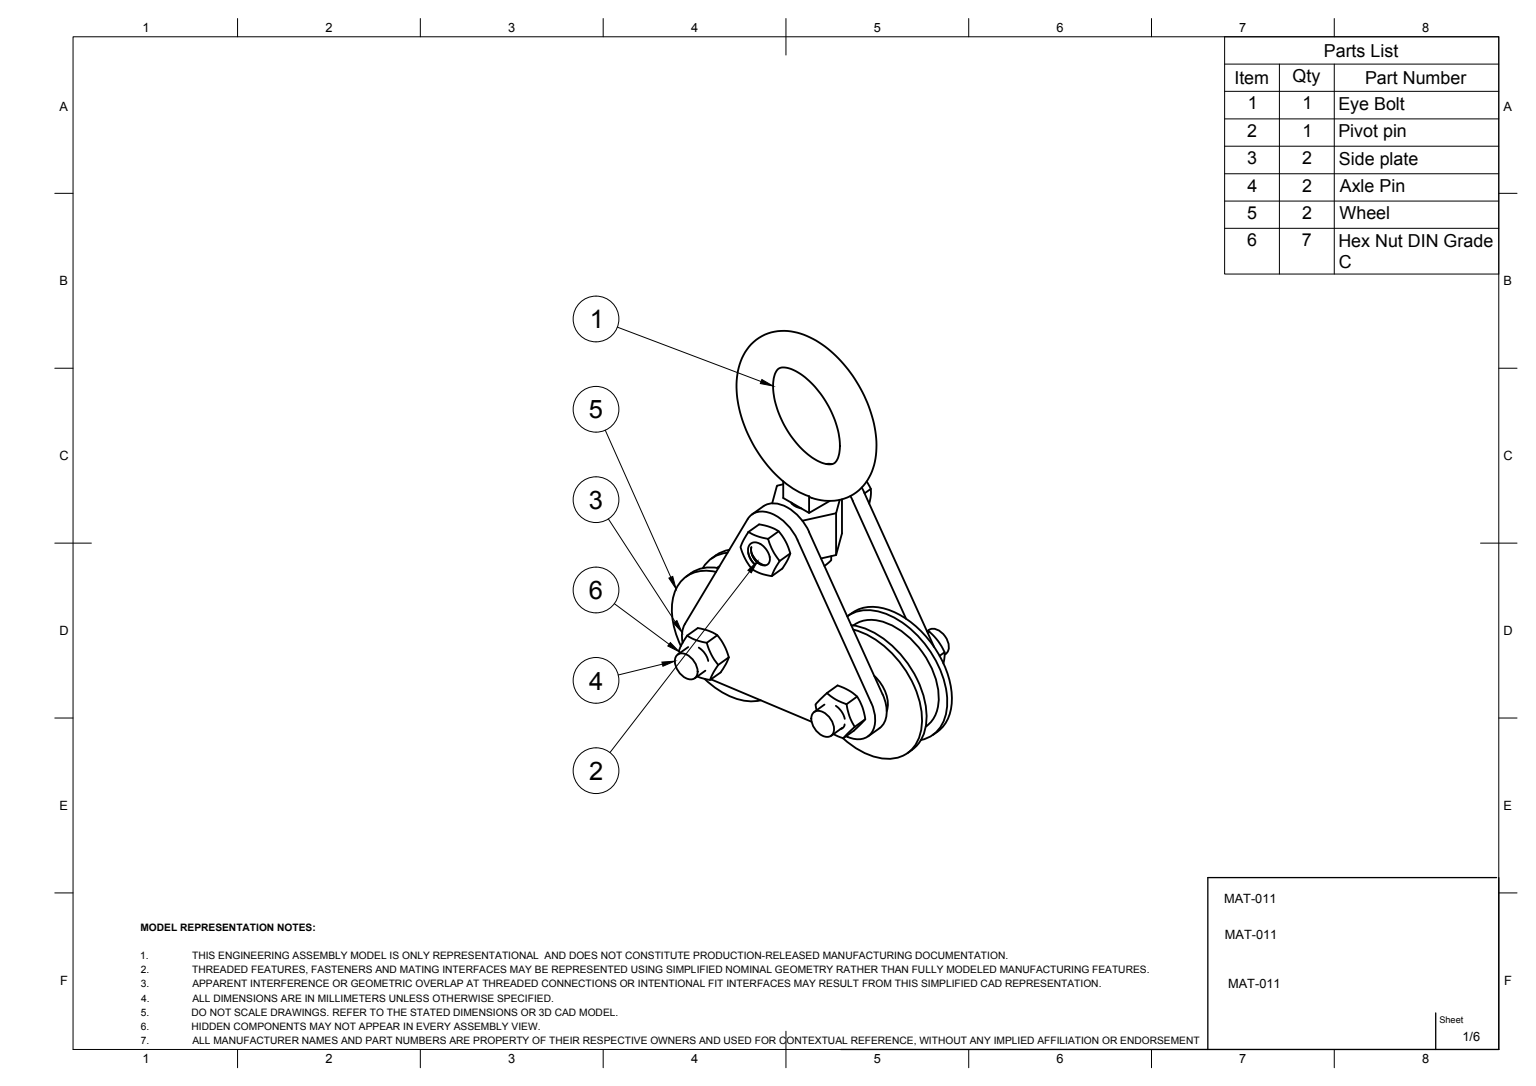
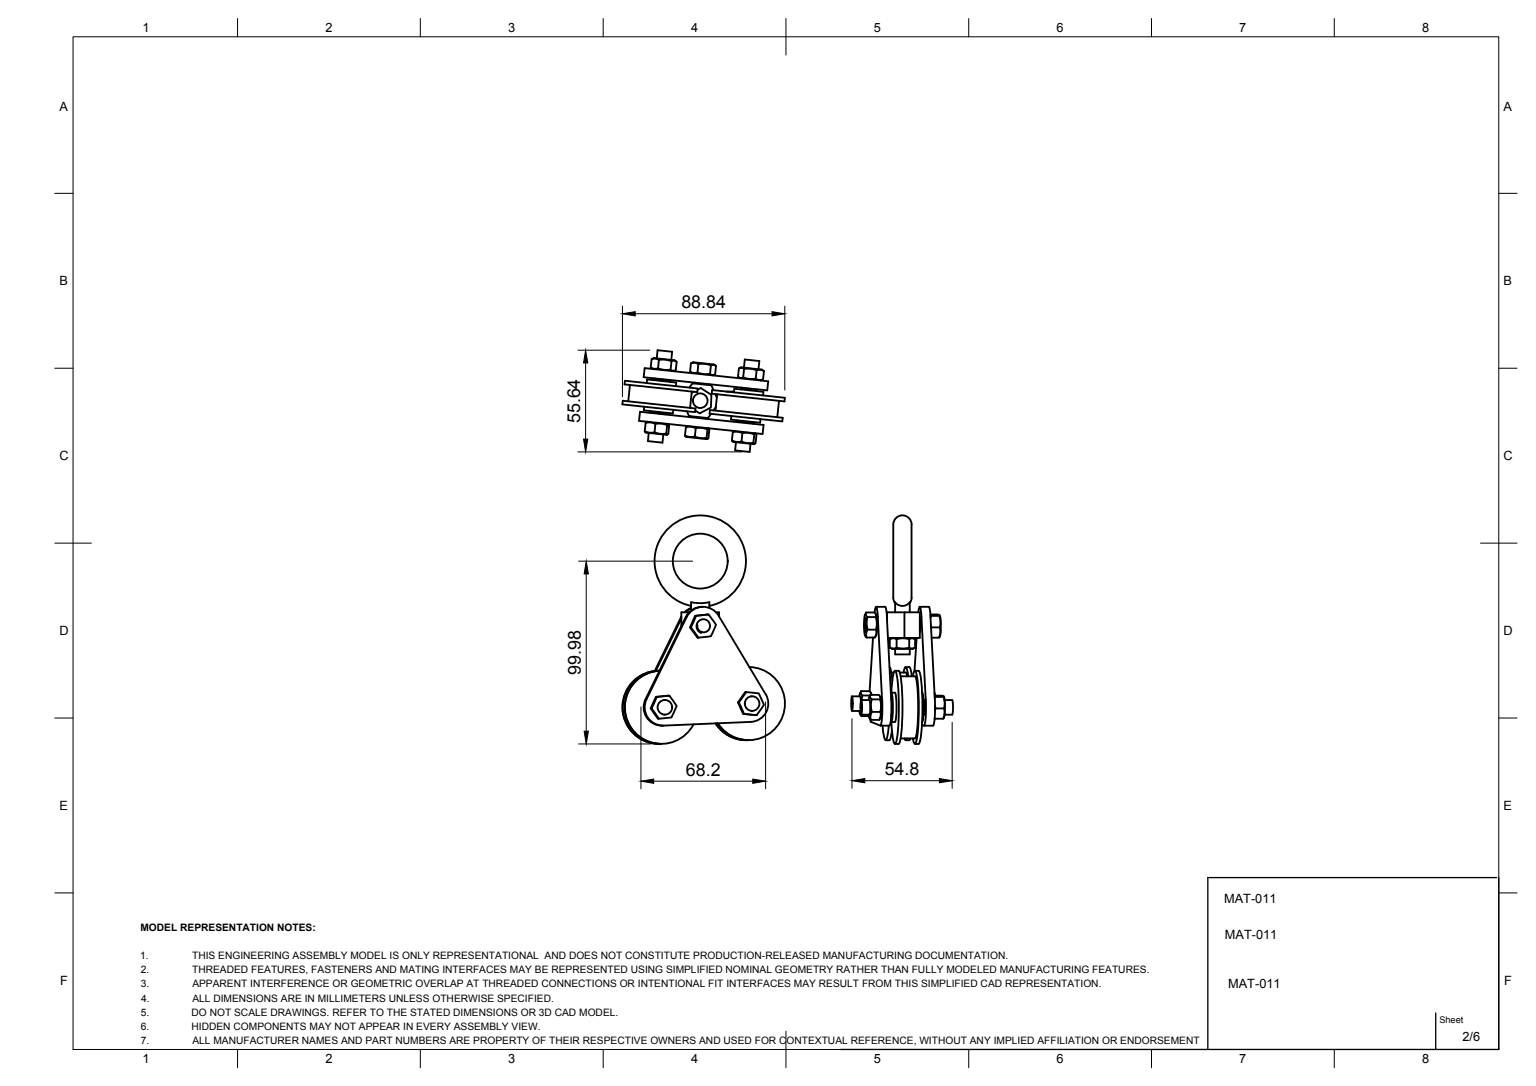
ISO-10303-21;
HEADER;
/* Generated by software containing ST-Developer
 * from STEP Tools, Inc. (www.steptools.com) 
 */

FILE_DESCRIPTION(
/* description */ ('STEP AP214'),
/* implementation_level */ '2;1');

FILE_NAME(
/* name */ 'MAT-011.step',
/* time_stamp */ '2026-11-14T05:56:09-08:00',
/* author */ (''),
/* organization */ (''),
/* preprocessor_version */ 'ST-DEVELOPER v20.2',
/* originating_system */ 'Autodesk Translation Framework v15.17.0.0',
/* authorisation */ '');

FILE_SCHEMA (('AUTOMOTIVE_DESIGN { 1 0 10303 214 3 1 1 }'));
ENDSEC;

DATA;
#10=MECHANICAL_DESIGN_GEOMETRIC_PRESENTATION_REPRESENTATION('',(#102,#103,
#104,#105,#106,#107),#3207);
#11=ITEM_DEFINED_TRANSFORMATION($,$,#1354,#1503);
#12=ITEM_DEFINED_TRANSFORMATION($,$,#1372,#1504);
#13=ITEM_DEFINED_TRANSFORMATION($,$,#1416,#1505);
#14=ITEM_DEFINED_TRANSFORMATION($,$,#1398,#1506);
#15=ITEM_DEFINED_TRANSFORMATION($,$,#1440,#1507);
#16=ITEM_DEFINED_TRANSFORMATION($,$,#1465,#1508);
#17=ITEM_DEFINED_TRANSFORMATION($,$,#1398,#1509);
#18=ITEM_DEFINED_TRANSFORMATION($,$,#1416,#1510);
#19=ITEM_DEFINED_TRANSFORMATION($,$,#1440,#1511);
#20=ITEM_DEFINED_TRANSFORMATION($,$,#1465,#1512);
#21=ITEM_DEFINED_TRANSFORMATION($,$,#1465,#1513);
#22=ITEM_DEFINED_TRANSFORMATION($,$,#1465,#1514);
#23=ITEM_DEFINED_TRANSFORMATION($,$,#1465,#1515);
#24=ITEM_DEFINED_TRANSFORMATION($,$,#1465,#1516);
#25=ITEM_DEFINED_TRANSFORMATION($,$,#1465,#1517);
#26=(
REPRESENTATION_RELATIONSHIP($,$,#3242,#3241)
REPRESENTATION_RELATIONSHIP_WITH_TRANSFORMATION(#11)
SHAPE_REPRESENTATION_RELATIONSHIP()
);
#27=(
REPRESENTATION_RELATIONSHIP($,$,#3243,#3241)
REPRESENTATION_RELATIONSHIP_WITH_TRANSFORMATION(#12)
SHAPE_REPRESENTATION_RELATIONSHIP()
);
#28=(
REPRESENTATION_RELATIONSHIP($,$,#3245,#3241)
REPRESENTATION_RELATIONSHIP_WITH_TRANSFORMATION(#13)
SHAPE_REPRESENTATION_RELATIONSHIP()
);
#29=(
REPRESENTATION_RELATIONSHIP($,$,#3244,#3241)
REPRESENTATION_RELATIONSHIP_WITH_TRANSFORMATION(#14)
SHAPE_REPRESENTATION_RELATIONSHIP()
);
#30=(
REPRESENTATION_RELATIONSHIP($,$,#3246,#3241)
REPRESENTATION_RELATIONSHIP_WITH_TRANSFORMATION(#15)
SHAPE_REPRESENTATION_RELATIONSHIP()
);
#31=(
REPRESENTATION_RELATIONSHIP($,$,#3247,#3241)
REPRESENTATION_RELATIONSHIP_WITH_TRANSFORMATION(#16)
SHAPE_REPRESENTATION_RELATIONSHIP()
);
#32=(
REPRESENTATION_RELATIONSHIP($,$,#3244,#3241)
REPRESENTATION_RELATIONSHIP_WITH_TRANSFORMATION(#17)
SHAPE_REPRESENTATION_RELATIONSHIP()
);
#33=(
REPRESENTATION_RELATIONSHIP($,$,#3245,#3241)
REPRESENTATION_RELATIONSHIP_WITH_TRANSFORMATION(#18)
SHAPE_REPRESENTATION_RELATIONSHIP()
);
#34=(
REPRESENTATION_RELATIONSHIP($,$,#3246,#3241)
REPRESENTATION_RELATIONSHIP_WITH_TRANSFORMATION(#19)
SHAPE_REPRESENTATION_RELATIONSHIP()
);
#35=(
REPRESENTATION_RELATIONSHIP($,$,#3247,#3241)
REPRESENTATION_RELATIONSHIP_WITH_TRANSFORMATION(#20)
SHAPE_REPRESENTATION_RELATIONSHIP()
);
#36=(
REPRESENTATION_RELATIONSHIP($,$,#3247,#3241)
REPRESENTATION_RELATIONSHIP_WITH_TRANSFORMATION(#21)
SHAPE_REPRESENTATION_RELATIONSHIP()
);
#37=(
REPRESENTATION_RELATIONSHIP($,$,#3247,#3241)
REPRESENTATION_RELATIONSHIP_WITH_TRANSFORMATION(#22)
SHAPE_REPRESENTATION_RELATIONSHIP()
);
#38=(
REPRESENTATION_RELATIONSHIP($,$,#3247,#3241)
REPRESENTATION_RELATIONSHIP_WITH_TRANSFORMATION(#23)
SHAPE_REPRESENTATION_RELATIONSHIP()
);
#39=(
REPRESENTATION_RELATIONSHIP($,$,#3247,#3241)
REPRESENTATION_RELATIONSHIP_WITH_TRANSFORMATION(#24)
SHAPE_REPRESENTATION_RELATIONSHIP()
);
#40=(
REPRESENTATION_RELATIONSHIP($,$,#3247,#3241)
REPRESENTATION_RELATIONSHIP_WITH_TRANSFORMATION(#25)
SHAPE_REPRESENTATION_RELATIONSHIP()
);
#41=CONTEXT_DEPENDENT_SHAPE_REPRESENTATION(#26,#3226);
#42=CONTEXT_DEPENDENT_SHAPE_REPRESENTATION(#27,#3227);
#43=CONTEXT_DEPENDENT_SHAPE_REPRESENTATION(#28,#3228);
#44=CONTEXT_DEPENDENT_SHAPE_REPRESENTATION(#29,#3229);
#45=CONTEXT_DEPENDENT_SHAPE_REPRESENTATION(#30,#3230);
#46=CONTEXT_DEPENDENT_SHAPE_REPRESENTATION(#31,#3231);
#47=CONTEXT_DEPENDENT_SHAPE_REPRESENTATION(#32,#3232);
#48=CONTEXT_DEPENDENT_SHAPE_REPRESENTATION(#33,#3233);
#49=CONTEXT_DEPENDENT_SHAPE_REPRESENTATION(#34,#3234);
#50=CONTEXT_DEPENDENT_SHAPE_REPRESENTATION(#35,#3235);
#51=CONTEXT_DEPENDENT_SHAPE_REPRESENTATION(#36,#3236);
#52=CONTEXT_DEPENDENT_SHAPE_REPRESENTATION(#37,#3237);
#53=CONTEXT_DEPENDENT_SHAPE_REPRESENTATION(#38,#3238);
#54=CONTEXT_DEPENDENT_SHAPE_REPRESENTATION(#39,#3239);
#55=CONTEXT_DEPENDENT_SHAPE_REPRESENTATION(#40,#3240);
#56=NEXT_ASSEMBLY_USAGE_OCCURRENCE('Eye Bolt:1','Eye Bolt:1',
'Eye Bolt:1',#3249,#3250,'Eye Bolt:1');
#57=NEXT_ASSEMBLY_USAGE_OCCURRENCE('Pivot Pin:1','Pivot Pin:1',
'Pivot Pin:1',#3249,#3251,'Pivot Pin:1');
#58=NEXT_ASSEMBLY_USAGE_OCCURRENCE('Side Plate:1','Side Plate:1',
'Side Plate:1',#3249,#3253,'Side Plate:1');
#59=NEXT_ASSEMBLY_USAGE_OCCURRENCE('Axle Pin:1','Axle Pin:1',
'Axle Pin:1',#3249,#3252,'Axle Pin:1');
#60=NEXT_ASSEMBLY_USAGE_OCCURRENCE('Wheel:1','Wheel:1','Wheel:1',#3249,
#3254,'Wheel:1');
#61=NEXT_ASSEMBLY_USAGE_OCCURRENCE('Hex Nut DIN Grade C:1',
'Hex Nut DIN Grade C:1','Hex Nut DIN Grade C:1',#3249,#3255,
'Hex Nut DIN Grade C:1');
#62=NEXT_ASSEMBLY_USAGE_OCCURRENCE('Axle Pin:2','Axle Pin:2',
'Axle Pin:2',#3249,#3252,'Axle Pin:2');
#63=NEXT_ASSEMBLY_USAGE_OCCURRENCE('Side Plate:2','Side Plate:2',
'Side Plate:2',#3249,#3253,'Side Plate:2');
#64=NEXT_ASSEMBLY_USAGE_OCCURRENCE('Wheel:2','Wheel:2','Wheel:2',#3249,
#3254,'Wheel:2');
#65=NEXT_ASSEMBLY_USAGE_OCCURRENCE('Hex Nut DIN Grade C:2',
'Hex Nut DIN Grade C:2','Hex Nut DIN Grade C:2',#3249,#3255,
'Hex Nut DIN Grade C:2');
#66=NEXT_ASSEMBLY_USAGE_OCCURRENCE('Hex Nut DIN Grade C:3',
'Hex Nut DIN Grade C:3','Hex Nut DIN Grade C:3',#3249,#3255,
'Hex Nut DIN Grade C:3');
#67=NEXT_ASSEMBLY_USAGE_OCCURRENCE('Hex Nut DIN Grade C:4',
'Hex Nut DIN Grade C:4','Hex Nut DIN Grade C:4',#3249,#3255,
'Hex Nut DIN Grade C:4');
#68=NEXT_ASSEMBLY_USAGE_OCCURRENCE('Hex Nut DIN Grade C:5',
'Hex Nut DIN Grade C:5','Hex Nut DIN Grade C:5',#3249,#3255,
'Hex Nut DIN Grade C:5');
#69=NEXT_ASSEMBLY_USAGE_OCCURRENCE('Hex Nut DIN Grade C:6',
'Hex Nut DIN Grade C:6','Hex Nut DIN Grade C:6',#3249,#3255,
'Hex Nut DIN Grade C:6');
#70=NEXT_ASSEMBLY_USAGE_OCCURRENCE('Hex Nut DIN Grade C:7',
'Hex Nut DIN Grade C:7','Hex Nut DIN Grade C:7',#3249,#3255,
'Hex Nut DIN Grade C:7');
#71=(
BOUNDED_SURFACE()
B_SPLINE_SURFACE(1,2,((#2712,#2713,#2714,#2715,#2716,#2717,#2718,#2719,
#2720,#2721,#2722,#2723,#2724,#2725,#2726,#2727,#2728,#2729,#2730,#2731,
#2732,#2733,#2734,#2735,#2736,#2737,#2738,#2739,#2740,#2741,#2742,#2743,
#2744,#2745,#2746,#2747,#2748,#2749,#2750,#2751,#2752,#2753,#2754,#2755,
#2756,#2757,#2758,#2759,#2760,#2761,#2762,#2763,#2764,#2765,#2766,#2767,
#2768,#2769,#2770,#2771,#2772,#2773,#2774,#2775,#2776,#2777,#2778,#2779,
#2780,#2781,#2782,#2783,#2784,#2785,#2786,#2787,#2788,#2789,#2790,#2791,
#2792,#2793,#2794,#2795,#2796,#2797,#2798,#2799,#2800,#2801,#2802,#2803,
#2804,#2805,#2806,#2807,#2808),(#2809,#2810,#2811,#2812,#2813,#2814,#2815,
#2816,#2817,#2818,#2819,#2820,#2821,#2822,#2823,#2824,#2825,#2826,#2827,
#2828,#2829,#2830,#2831,#2832,#2833,#2834,#2835,#2836,#2837,#2838,#2839,
#2840,#2841,#2842,#2843,#2844,#2845,#2846,#2847,#2848,#2849,#2850,#2851,
#2852,#2853,#2854,#2855,#2856,#2857,#2858,#2859,#2860,#2861,#2862,#2863,
#2864,#2865,#2866,#2867,#2868,#2869,#2870,#2871,#2872,#2873,#2874,#2875,
#2876,#2877,#2878,#2879,#2880,#2881,#2882,#2883,#2884,#2885,#2886,#2887,
#2888,#2889,#2890,#2891,#2892,#2893,#2894,#2895,#2896,#2897,#2898,#2899,
#2900,#2901,#2902,#2903,#2904,#2905)),.UNSPECIFIED.,.F.,.F.,.F.)
B_SPLINE_SURFACE_WITH_KNOTS((2,2),(3,2,2,2,2,2,2,2,2,2,2,2,2,2,2,2,2,2,
2,2,2,2,2,2,2,2,2,2,2,2,2,2,2,2,2,2,2,2,2,2,2,2,2,2,2,2,2,2,3),(0.,1.),
(0.,0.0208333333333333,0.0416666666666667,0.0625,0.0833333333333333,0.104166666666667,
0.125,0.145833333333333,0.166666666666667,0.1875,0.208333333333333,0.229166666666667,
0.25,0.270833333333333,0.291666666666667,0.3125,0.333333333333333,0.354166666666667,
0.375,0.395833333333333,0.416666666666667,0.4375,0.458333333333333,0.479166666666667,
0.5,0.520833333333333,0.541666666666667,0.5625,0.583333333333333,0.604166666666667,
0.625,0.645833333333333,0.666666666666667,0.6875,0.708333333333333,0.729166666666667,
0.75,0.770833333333333,0.791666666666667,0.8125,0.833333333333333,0.854166666666667,
0.875,0.895833333333333,0.916666666666667,0.9375,0.958333333333333,0.979166666666667,
1.),.UNSPECIFIED.)
GEOMETRIC_REPRESENTATION_ITEM()
RATIONAL_B_SPLINE_SURFACE(((1.,0.923879532511287,1.,0.923879532511287,1.,
0.923879532511287,1.,0.923879532511287,1.,0.923879532511287,1.,0.923879532511287,
1.,0.923879532511287,1.,0.923879532511287,1.,0.923879532511287,1.,0.923879532511287,
1.,0.923879532511287,1.,0.923879532511287,1.,0.923879532511287,1.,0.923879532511287,
1.,0.923879532511287,1.,0.923879532511287,1.,0.923879532511287,1.,0.923879532511287,
1.,0.923879532511287,1.,0.923879532511287,1.,0.923879532511287,1.,0.923879532511287,
1.,0.923879532511287,1.,0.923879532511287,1.,0.923879532511287,1.,0.923879532511287,
1.,0.923879532511287,1.,0.923879532511287,1.,0.923879532511287,1.,0.923879532511287,
1.,0.923879532511287,1.,0.923879532511287,1.,0.923879532511287,1.,0.923879532511287,
1.,0.923879532511287,1.,0.923879532511287,1.,0.923879532511287,1.,0.923879532511287,
1.,0.923879532511287,1.,0.923879532511287,1.,0.923879532511287,1.,0.923879532511287,
1.,0.923879532511287,1.,0.923879532511287,1.,0.923879532511287,1.,0.923879532511287,
1.,0.923879532511287,1.,0.923879532511287,1.),(1.,0.923879532511287,1.,
0.923879532511287,1.,0.923879532511287,1.,0.923879532511287,1.,0.923879532511287,
1.,0.923879532511287,1.,0.923879532511287,1.,0.923879532511287,1.,0.923879532511287,
1.,0.923879532511287,1.,0.923879532511287,1.,0.923879532511287,1.,0.923879532511287,
1.,0.923879532511287,1.,0.923879532511287,1.,0.923879532511287,1.,0.923879532511287,
1.,0.923879532511287,1.,0.923879532511287,1.,0.923879532511287,1.,0.923879532511287,
1.,0.923879532511287,1.,0.923879532511287,1.,0.923879532511287,1.,0.923879532511287,
1.,0.923879532511287,1.,0.923879532511287,1.,0.923879532511287,1.,0.923879532511287,
1.,0.923879532511287,1.,0.923879532511287,1.,0.923879532511287,1.,0.923879532511287,
1.,0.923879532511287,1.,0.923879532511287,1.,0.923879532511287,1.,0.923879532511287,
1.,0.923879532511287,1.,0.923879532511287,1.,0.923879532511287,1.,0.923879532511287,
1.,0.923879532511287,1.,0.923879532511287,1.,0.923879532511287,1.,0.923879532511287,
1.,0.923879532511287,1.,0.923879532511287,1.,0.923879532511287,1.)))
REPRESENTATION_ITEM('')
SURFACE()
);
#72=(
BOUNDED_SURFACE()
B_SPLINE_SURFACE(1,2,((#2983,#2984,#2985,#2986,#2987,#2988,#2989,#2990,
#2991,#2992,#2993,#2994,#2995,#2996,#2997,#2998,#2999,#3000,#3001,#3002,
#3003,#3004,#3005,#3006,#3007,#3008,#3009,#3010,#3011,#3012,#3013,#3014,
#3015,#3016,#3017,#3018,#3019,#3020,#3021,#3022,#3023,#3024,#3025,#3026,
#3027,#3028,#3029,#3030,#3031,#3032,#3033,#3034,#3035,#3036,#3037,#3038,
#3039,#3040,#3041,#3042,#3043,#3044,#3045,#3046,#3047,#3048,#3049,#3050,
#3051,#3052,#3053,#3054,#3055,#3056,#3057,#3058,#3059,#3060,#3061,#3062,
#3063,#3064,#3065,#3066,#3067,#3068,#3069,#3070,#3071,#3072,#3073,#3074,
#3075,#3076,#3077,#3078,#3079),(#3080,#3081,#3082,#3083,#3084,#3085,#3086,
#3087,#3088,#3089,#3090,#3091,#3092,#3093,#3094,#3095,#3096,#3097,#3098,
#3099,#3100,#3101,#3102,#3103,#3104,#3105,#3106,#3107,#3108,#3109,#3110,
#3111,#3112,#3113,#3114,#3115,#3116,#3117,#3118,#3119,#3120,#3121,#3122,
#3123,#3124,#3125,#3126,#3127,#3128,#3129,#3130,#3131,#3132,#3133,#3134,
#3135,#3136,#3137,#3138,#3139,#3140,#3141,#3142,#3143,#3144,#3145,#3146,
#3147,#3148,#3149,#3150,#3151,#3152,#3153,#3154,#3155,#3156,#3157,#3158,
#3159,#3160,#3161,#3162,#3163,#3164,#3165,#3166,#3167,#3168,#3169,#3170,
#3171,#3172,#3173,#3174,#3175,#3176)),.UNSPECIFIED.,.F.,.F.,.F.)
B_SPLINE_SURFACE_WITH_KNOTS((2,2),(3,2,2,2,2,2,2,2,2,2,2,2,2,2,2,2,2,2,
2,2,2,2,2,2,2,2,2,2,2,2,2,2,2,2,2,2,2,2,2,2,2,2,2,2,2,2,2,2,3),(0.,1.00006669780522),
(0.,0.0208333333333333,0.0416666666666667,0.0625,0.0833333333333333,0.104166666666667,
0.125,0.145833333333333,0.166666666666667,0.1875,0.208333333333333,0.229166666666667,
0.25,0.270833333333333,0.291666666666667,0.3125,0.333333333333333,0.354166666666667,
0.375,0.395833333333333,0.416666666666667,0.4375,0.458333333333333,0.479166666666667,
0.5,0.520833333333333,0.541666666666667,0.5625,0.583333333333333,0.604166666666667,
0.625,0.645833333333333,0.666666666666667,0.6875,0.708333333333333,0.729166666666667,
0.75,0.770833333333333,0.791666666666667,0.8125,0.833333333333333,0.854166666666667,
0.875,0.895833333333333,0.916666666666667,0.9375,0.958333333333333,0.979166666666667,
1.),.UNSPECIFIED.)
GEOMETRIC_REPRESENTATION_ITEM()
RATIONAL_B_SPLINE_SURFACE(((1.,0.923879532511287,1.,0.923879532511287,1.,
0.923879532511287,1.,0.923879532511287,1.,0.923879532511287,1.,0.923879532511287,
1.,0.923879532511287,1.,0.923879532511287,1.,0.923879532511287,1.,0.923879532511287,
1.,0.923879532511287,1.,0.923879532511287,1.,0.923879532511287,1.,0.923879532511287,
1.,0.923879532511287,1.,0.923879532511287,1.,0.923879532511287,1.,0.923879532511287,
1.,0.923879532511287,1.,0.923879532511287,1.,0.923879532511287,1.,0.923879532511287,
1.,0.923879532511287,1.,0.923879532511287,1.,0.923879532511287,1.,0.923879532511287,
1.,0.923879532511287,1.,0.923879532511287,1.,0.923879532511287,1.,0.923879532511287,
1.,0.923879532511287,1.,0.923879532511287,1.,0.923879532511287,1.,0.923879532511287,
1.,0.923879532511287,1.,0.923879532511287,1.,0.923879532511287,1.,0.923879532511287,
1.,0.923879532511287,1.,0.923879532511287,1.,0.923879532511287,1.,0.923879532511287,
1.,0.923879532511287,1.,0.923879532511287,1.,0.923879532511287,1.,0.923879532511287,
1.,0.923879532511287,1.,0.923879532511287,1.),(1.,0.923879532511287,1.,
0.923879532511287,1.,0.923879532511287,1.,0.923879532511287,1.,0.923879532511287,
1.,0.923879532511287,1.,0.923879532511287,1.,0.923879532511287,1.,0.923879532511287,
1.,0.923879532511287,1.,0.923879532511287,1.,0.923879532511287,1.,0.923879532511287,
1.,0.923879532511287,1.,0.923879532511287,1.,0.923879532511287,1.,0.923879532511287,
1.,0.923879532511287,1.,0.923879532511287,1.,0.923879532511287,1.,0.923879532511287,
1.,0.923879532511287,1.,0.923879532511287,1.,0.923879532511287,1.,0.923879532511287,
1.,0.923879532511287,1.,0.923879532511287,1.,0.923879532511287,1.,0.923879532511287,
1.,0.923879532511287,1.,0.923879532511287,1.,0.923879532511287,1.,0.923879532511287,
1.,0.923879532511287,1.,0.923879532511287,1.,0.923879532511287,1.,0.923879532511287,
1.,0.923879532511287,1.,0.923879532511287,1.,0.923879532511287,1.,0.923879532511287,
1.,0.923879532511287,1.,0.923879532511287,1.,0.923879532511287,1.,0.923879532511287,
1.,0.923879532511287,1.,0.923879532511287,1.,0.923879532511287,1.)))
REPRESENTATION_ITEM('')
SURFACE()
);
#73=(
BOUNDED_CURVE()
B_SPLINE_CURVE(2,(#2576,#2577,#2578),.UNSPECIFIED.,.F.,.F.)
B_SPLINE_CURVE_WITH_KNOTS((3,3),(-2.54218368144079,-1.15030563525544),
 .UNSPECIFIED.)
CURVE()
GEOMETRIC_REPRESENTATION_ITEM()
RATIONAL_B_SPLINE_CURVE((1.87625870439026,2.16651693610016,1.87625870439027))
REPRESENTATION_ITEM('')
);
#74=(
BOUNDED_CURVE()
B_SPLINE_CURVE(2,(#2580,#2581,#2582),.UNSPECIFIED.,.F.,.F.)
B_SPLINE_CURVE_WITH_KNOTS((3,3),(-2.54218475501031,-1.15030626839472),
 .UNSPECIFIED.)
CURVE()
GEOMETRIC_REPRESENTATION_ITEM()
RATIONAL_B_SPLINE_CURVE((1.87625926314051,2.16651758128937,1.87625926314051))
REPRESENTATION_ITEM('')
);
#75=(
BOUNDED_CURVE()
B_SPLINE_CURVE(2,(#2584,#2585,#2586),.UNSPECIFIED.,.F.,.F.)
B_SPLINE_CURVE_WITH_KNOTS((3,3),(-2.54218368144076,-1.15030563525543),
 .UNSPECIFIED.)
CURVE()
GEOMETRIC_REPRESENTATION_ITEM()
RATIONAL_B_SPLINE_CURVE((1.87625870439026,2.16651693610015,1.87625870439025))
REPRESENTATION_ITEM('')
);
#76=(
BOUNDED_CURVE()
B_SPLINE_CURVE(2,(#2589,#2590,#2591),.UNSPECIFIED.,.F.,.F.)
B_SPLINE_CURVE_WITH_KNOTS((3,3),(1.15030563525545,2.54218368144079),
 .UNSPECIFIED.)
CURVE()
GEOMETRIC_REPRESENTATION_ITEM()
RATIONAL_B_SPLINE_CURVE((1.87625870439026,2.16651693610015,1.87625870439025))
REPRESENTATION_ITEM('')
);
#77=(
BOUNDED_CURVE()
B_SPLINE_CURVE(2,(#2593,#2594,#2595),.UNSPECIFIED.,.F.,.F.)
B_SPLINE_CURVE_WITH_KNOTS((3,3),(1.15030626839473,2.54218475501033),
 .UNSPECIFIED.)
CURVE()
GEOMETRIC_REPRESENTATION_ITEM()
RATIONAL_B_SPLINE_CURVE((1.87625926314051,2.16651758128937,1.8762592631405))
REPRESENTATION_ITEM('')
);
#78=(
BOUNDED_CURVE()
B_SPLINE_CURVE(2,(#2596,#2597,#2598),.UNSPECIFIED.,.F.,.F.)
B_SPLINE_CURVE_WITH_KNOTS((3,3),(1.15030563525543,2.54218368144081),
 .UNSPECIFIED.)
CURVE()
GEOMETRIC_REPRESENTATION_ITEM()
RATIONAL_B_SPLINE_CURVE((1.87625870439027,2.16651693610019,1.87625870439027))
REPRESENTATION_ITEM('')
);
#79=(
BOUNDED_CURVE()
B_SPLINE_CURVE(2,(#2602,#2603,#2604),.UNSPECIFIED.,.F.,.F.)
B_SPLINE_CURVE_WITH_KNOTS((3,3),(-2.66143679957435,-1.22056556713595),
 .UNSPECIFIED.)
CURVE()
GEOMETRIC_REPRESENTATION_ITEM()
RATIONAL_B_SPLINE_CURVE((1.93841739578654,2.23829161052161,1.93841739578655))
REPRESENTATION_ITEM('')
);
#80=(
BOUNDED_CURVE()
B_SPLINE_CURVE(2,(#2606,#2607,#2608),.UNSPECIFIED.,.F.,.F.)
B_SPLINE_CURVE_WITH_KNOTS((3,3),(-2.66143679957435,-1.22056556713593),
 .UNSPECIFIED.)
CURVE()
GEOMETRIC_REPRESENTATION_ITEM()
RATIONAL_B_SPLINE_CURVE((1.93841739578655,2.23829161052162,1.93841739578654))
REPRESENTATION_ITEM('')
);
#81=(
BOUNDED_CURVE()
B_SPLINE_CURVE(2,(#2610,#2611,#2612),.UNSPECIFIED.,.F.,.F.)
B_SPLINE_CURVE_WITH_KNOTS((3,3),(-2.66143679957436,-1.22056556713593),
 .UNSPECIFIED.)
CURVE()
GEOMETRIC_REPRESENTATION_ITEM()
RATIONAL_B_SPLINE_CURVE((1.93841739578655,2.23829161052163,1.93841739578654))
REPRESENTATION_ITEM('')
);
#82=(
BOUNDED_CURVE()
B_SPLINE_CURVE(2,(#2615,#2616,#2617),.UNSPECIFIED.,.F.,.F.)
B_SPLINE_CURVE_WITH_KNOTS((3,3),(1.22056556713593,2.66143679957439),
 .UNSPECIFIED.)
CURVE()
GEOMETRIC_REPRESENTATION_ITEM()
RATIONAL_B_SPLINE_CURVE((1.93841739578656,2.23829161052165,1.93841739578656))
REPRESENTATION_ITEM('')
);
#83=(
BOUNDED_CURVE()
B_SPLINE_CURVE(2,(#2619,#2620,#2621),.UNSPECIFIED.,.F.,.F.)
B_SPLINE_CURVE_WITH_KNOTS((3,3),(1.22056556713592,2.66143679957436),
 .UNSPECIFIED.)
CURVE()
GEOMETRIC_REPRESENTATION_ITEM()
RATIONAL_B_SPLINE_CURVE((1.93841739578654,2.23829161052163,1.93841739578655))
REPRESENTATION_ITEM('')
);
#84=(
BOUNDED_CURVE()
B_SPLINE_CURVE(2,(#2622,#2623,#2624),.UNSPECIFIED.,.F.,.F.)
B_SPLINE_CURVE_WITH_KNOTS((3,3),(1.22056556713592,2.66143679957434),
 .UNSPECIFIED.)
CURVE()
GEOMETRIC_REPRESENTATION_ITEM()
RATIONAL_B_SPLINE_CURVE((1.93841739578653,2.23829161052161,1.93841739578655))
REPRESENTATION_ITEM('')
);
#85=(
BOUNDED_CURVE()
B_SPLINE_CURVE(2,(#2906,#2907,#2908,#2909,#2910,#2911,#2912,#2913,#2914,
#2915,#2916,#2917,#2918,#2919,#2920,#2921,#2922,#2923,#2924,#2925,#2926,
#2927,#2928,#2929,#2930,#2931,#2932,#2933,#2934,#2935,#2936,#2937,#2938,
#2939,#2940,#2941,#2942,#2943,#2944,#2945,#2946,#2947,#2948,#2949,#2950,
#2951,#2952,#2953,#2954,#2955,#2956,#2957,#2958,#2959,#2960,#2961,#2962,
#2963,#2964,#2965,#2966,#2967,#2968,#2969,#2970,#2971,#2972,#2973,#2974,
#2975,#2976,#2977,#2978,#2979,#2980,#2981,#2982),.UNSPECIFIED.,.F.,.F.)
B_SPLINE_CURVE_WITH_KNOTS((3,2,2,2,2,2,2,2,2,2,2,2,2,2,2,2,2,2,2,2,2,2,
2,2,2,2,2,2,2,2,2,2,2,2,2,2,2,2,3),(0.0966194075737784,0.104166666666667,
0.125,0.145833333333333,0.166666666666667,0.1875,0.208333333333333,0.229166666666667,
0.25,0.270833333333333,0.291666666666667,0.3125,0.333333333333333,0.354166666666667,
0.375,0.395833333333333,0.416666666666667,0.4375,0.458333333333333,0.479166666666667,
0.5,0.520833333333333,0.541666666666667,0.5625,0.583333333333333,0.604166666666667,
0.625,0.645833333333333,0.666666666666667,0.6875,0.708333333333333,0.729166666666667,
0.75,0.770833333333333,0.791666666666667,0.8125,0.833333333333333,0.854166666666667,
0.868477508058086),.UNSPECIFIED.)
CURVE()
GEOMETRIC_REPRESENTATION_ITEM()
RATIONAL_B_SPLINE_CURVE((0.964827774294736,0.972423957260363,1.,0.923879532511287,
1.,0.923879532511287,1.,0.923879532511287,1.,0.923879532511287,1.,0.923879532511287,
1.,0.923879532511287,1.,0.923879532511287,1.,0.923879532511287,1.,0.923879532511287,
1.,0.923879532511287,1.,0.923879532511287,1.,0.923879532511287,1.,0.923879532511287,
1.,0.923879532511287,1.,0.923879532511287,1.,0.923879532511287,1.,0.923879532511287,
1.,0.923879532511287,1.,0.923879532511287,1.,0.923879532511287,1.,0.923879532511287,
1.,0.923879532511287,1.,0.923879532511287,1.,0.923879532511287,1.,0.923879532511287,
1.,0.923879532511287,1.,0.923879532511287,1.,0.923879532511287,1.,0.923879532511287,
1.,0.923879532511287,1.,0.923879532511287,1.,0.923879532511287,1.,0.923879532511287,
1.,0.923879532511287,1.,0.923879532511287,1.,0.923879532511287,1.,0.94771129903016,
0.967258947450023))
REPRESENTATION_ITEM('')
);
#86=CONICAL_SURFACE('',#1490,3.4,0.785398163397449);
#87=CONICAL_SURFACE('',#1491,4.1,0.785398163397447);
#88=CONICAL_SURFACE('',#1492,5.62820323027547,1.07685495787532);
#89=CONICAL_SURFACE('',#1493,6.92820323027547,1.07685495787532);
#90=SHAPE_REPRESENTATION_RELATIONSHIP('SRR','None',#3242,#96);
#91=SHAPE_REPRESENTATION_RELATIONSHIP('SRR','None',#3243,#97);
#92=SHAPE_REPRESENTATION_RELATIONSHIP('SRR','None',#3244,#98);
#93=SHAPE_REPRESENTATION_RELATIONSHIP('SRR','None',#3245,#99);
#94=SHAPE_REPRESENTATION_RELATIONSHIP('SRR','None',#3246,#100);
#95=SHAPE_REPRESENTATION_RELATIONSHIP('SRR','None',#3247,#101);
#96=ADVANCED_BREP_SHAPE_REPRESENTATION('',(#108),#3201);
#97=ADVANCED_BREP_SHAPE_REPRESENTATION('',(#109),#3202);
#98=ADVANCED_BREP_SHAPE_REPRESENTATION('',(#110),#3203);
#99=ADVANCED_BREP_SHAPE_REPRESENTATION('',(#111),#3204);
#100=ADVANCED_BREP_SHAPE_REPRESENTATION('',(#112),#3205);
#101=ADVANCED_BREP_SHAPE_REPRESENTATION('',(#113),#3206);
#102=STYLED_ITEM('',(#3281),#108);
#103=STYLED_ITEM('',(#3282),#109);
#104=STYLED_ITEM('',(#3281),#110);
#105=STYLED_ITEM('',(#3281),#111);
#106=STYLED_ITEM('',(#3282),#112);
#107=STYLED_ITEM('',(#3283),#113);
#108=MANIFOLD_SOLID_BREP('Body1',#1280);
#109=MANIFOLD_SOLID_BREP('Body1',#1281);
#110=MANIFOLD_SOLID_BREP('Body1',#1282);
#111=MANIFOLD_SOLID_BREP('Body1',#1283);
#112=MANIFOLD_SOLID_BREP('Body1',#1284);
#113=MANIFOLD_SOLID_BREP('Body1',#1285);
#114=PLANE('',#1365);
#115=PLANE('',#1366);
#116=PLANE('',#1367);
#117=PLANE('',#1368);
#118=PLANE('',#1369);
#119=PLANE('',#1370);
#120=PLANE('',#1371);
#121=PLANE('',#1388);
#122=PLANE('',#1389);
#123=PLANE('',#1390);
#124=PLANE('',#1391);
#125=PLANE('',#1392);
#126=PLANE('',#1393);
#127=PLANE('',#1394);
#128=PLANE('',#1395);
#129=PLANE('',#1396);
#130=PLANE('',#1397);
#131=PLANE('',#1414);
#132=PLANE('',#1415);
#133=PLANE('',#1429);
#134=PLANE('',#1432);
#135=PLANE('',#1435);
#136=PLANE('',#1437);
#137=PLANE('',#1439);
#138=PLANE('',#1459);
#139=PLANE('',#1460);
#140=PLANE('',#1461);
#141=PLANE('',#1462);
#142=PLANE('',#1463);
#143=PLANE('',#1464);
#144=PLANE('',#1495);
#145=PLANE('',#1496);
#146=PLANE('',#1497);
#147=PLANE('',#1498);
#148=PLANE('',#1499);
#149=PLANE('',#1500);
#150=PLANE('',#1501);
#151=PLANE('',#1502);
#152=LINE('',#1980,#219);
#153=LINE('',#1985,#220);
#154=LINE('',#1987,#221);
#155=LINE('',#1988,#222);
#156=LINE('',#1991,#223);
#157=LINE('',#1993,#224);
#158=LINE('',#1994,#225);
#159=LINE('',#1996,#226);
#160=LINE('',#1997,#227);
#161=LINE('',#1999,#228);
#162=LINE('',#2001,#229);
#163=LINE('',#2019,#230);
#164=LINE('',#2023,#231);
#165=LINE('',#2029,#232);
#166=LINE('',#2034,#233);
#167=LINE('',#2036,#234);
#168=LINE('',#2038,#235);
#169=LINE('',#2039,#236);
#170=LINE('',#2043,#237);
#171=LINE('',#2045,#238);
#172=LINE('',#2047,#239);
#173=LINE('',#2048,#240);
#174=LINE('',#2051,#241);
#175=LINE('',#2052,#242);
#176=LINE('',#2054,#243);
#177=LINE('',#2055,#244);
#178=LINE('',#2058,#245);
#179=LINE('',#2060,#246);
#180=LINE('',#2061,#247);
#181=LINE('',#2062,#248);
#182=LINE('',#2064,#249);
#183=LINE('',#2067,#250);
#184=LINE('',#2091,#251);
#185=LINE('',#2093,#252);
#186=LINE('',#2096,#253);
#187=LINE('',#2105,#254);
#188=LINE('',#2111,#255);
#189=LINE('',#2117,#256);
#190=LINE('',#2124,#257);
#191=LINE('',#2127,#258);
#192=LINE('',#2130,#259);
#193=LINE('',#2134,#260);
#194=LINE('',#2137,#261);
#195=LINE('',#2140,#262);
#196=LINE('',#2144,#263);
#197=LINE('',#2147,#264);
#198=LINE('',#2149,#265);
#199=LINE('',#2151,#266);
#200=LINE('',#2153,#267);
#201=LINE('',#2155,#268);
#202=LINE('',#2162,#269);
#203=LINE('',#2168,#270);
#204=LINE('',#2174,#271);
#205=LINE('',#2180,#272);
#206=LINE('',#2186,#273);
#207=LINE('',#2192,#274);
#208=LINE('',#2204,#275);
#209=LINE('',#2283,#276);
#210=LINE('',#2359,#277);
#211=LINE('',#2587,#278);
#212=LINE('',#2613,#279);
#213=LINE('',#2701,#280);
#214=LINE('',#2702,#281);
#215=LINE('',#2704,#282);
#216=LINE('',#2706,#283);
#217=LINE('',#2708,#284);
#218=LINE('',#2710,#285);
#219=VECTOR('',#1538,4.);
#220=VECTOR('',#1545,1000.);
#221=VECTOR('',#1546,1000.);
#222=VECTOR('',#1547,1000.);
#223=VECTOR('',#1550,1000.);
#224=VECTOR('',#1551,1000.);
#225=VECTOR('',#1552,1000.);
#226=VECTOR('',#1555,1000.);
#227=VECTOR('',#1556,1000.);
#228=VECTOR('',#1559,1000.);
#229=VECTOR('',#1562,1000.);
#230=VECTOR('',#1587,4.);
#231=VECTOR('',#1592,4.);
#232=VECTOR('',#1599,4.5);
#233=VECTOR('',#1604,1000.);
#234=VECTOR('',#1605,1000.);
#235=VECTOR('',#1606,1000.);
#236=VECTOR('',#1607,1000.);
#237=VECTOR('',#1610,1000.);
#238=VECTOR('',#1611,1000.);
#239=VECTOR('',#1612,1000.);
#240=VECTOR('',#1613,1000.);
#241=VECTOR('',#1616,1000.);
#242=VECTOR('',#1617,1000.);
#243=VECTOR('',#1618,1000.);
#244=VECTOR('',#1619,1000.);
#245=VECTOR('',#1622,1000.);
#246=VECTOR('',#1623,1000.);
#247=VECTOR('',#1624,1000.);
#248=VECTOR('',#1625,1000.);
#249=VECTOR('',#1628,1000.);
#250=VECTOR('',#1633,1000.);
#251=VECTOR('',#1666,4.);
#252=VECTOR('',#1669,4.5);
#253=VECTOR('',#1672,4.);
#254=VECTOR('',#1685,4.);
#255=VECTOR('',#1692,4.);
#256=VECTOR('',#1699,4.);
#257=VECTOR('',#1706,1000.);
#258=VECTOR('',#1709,1000.);
#259=VECTOR('',#1712,1000.);
#260=VECTOR('',#1715,1000.);
#261=VECTOR('',#1718,1000.);
#262=VECTOR('',#1721,1000.);
#263=VECTOR('',#1724,1000.);
#264=VECTOR('',#1727,1000.);
#265=VECTOR('',#1730,1000.);
#266=VECTOR('',#1733,1000.);
#267=VECTOR('',#1736,1000.);
#268=VECTOR('',#1739,1000.);
#269=VECTOR('',#1748,8.);
#270=VECTOR('',#1755,20.);
#271=VECTOR('',#1762,17.);
#272=VECTOR('',#1769,20.);
#273=VECTOR('',#1776,8.);
#274=VECTOR('',#1783,4.5);
#275=VECTOR('',#1802,3.4);
#276=VECTOR('',#1807,3.4);
#277=VECTOR('',#1810,3.4);
#278=VECTOR('',#1857,5.62820323027547);
#279=VECTOR('',#1860,6.92820323027547);
#280=VECTOR('',#1869,1000.);
#281=VECTOR('',#1870,1000.);
#282=VECTOR('',#1873,1000.);
#283=VECTOR('',#1876,1000.);
#284=VECTOR('',#1879,1000.);
#285=VECTOR('',#1882,1000.);
#286=CYLINDRICAL_SURFACE('',#1360,4.);
#287=CYLINDRICAL_SURFACE('',#1381,4.);
#288=CYLINDRICAL_SURFACE('',#1383,4.);
#289=CYLINDRICAL_SURFACE('',#1385,4.5);
#290=CYLINDRICAL_SURFACE('',#1409,4.);
#291=CYLINDRICAL_SURFACE('',#1411,4.5);
#292=CYLINDRICAL_SURFACE('',#1412,4.);
#293=CYLINDRICAL_SURFACE('',#1417,4.);
#294=CYLINDRICAL_SURFACE('',#1420,4.);
#295=CYLINDRICAL_SURFACE('',#1423,4.);
#296=CYLINDRICAL_SURFACE('',#1426,10.);
#297=CYLINDRICAL_SURFACE('',#1436,9.99999951505478);
#298=CYLINDRICAL_SURFACE('',#1438,10.);
#299=CYLINDRICAL_SURFACE('',#1441,8.);
#300=CYLINDRICAL_SURFACE('',#1444,20.);
#301=CYLINDRICAL_SURFACE('',#1447,17.);
#302=CYLINDRICAL_SURFACE('',#1450,20.);
#303=CYLINDRICAL_SURFACE('',#1453,8.);
#304=CYLINDRICAL_SURFACE('',#1456,4.5);
#305=CYLINDRICAL_SURFACE('',#1466,3.4);
#306=CYLINDRICAL_SURFACE('',#1468,3.4);
#307=CYLINDRICAL_SURFACE('',#1469,3.4);
#308=CYLINDRICAL_SURFACE('',#1494,3.4);
#309=FACE_BOUND('',#423,.T.);
#310=FACE_BOUND('',#438,.T.);
#311=FACE_BOUND('',#440,.T.);
#312=FACE_BOUND('',#442,.T.);
#313=FACE_BOUND('',#444,.T.);
#314=FACE_BOUND('',#463,.T.);
#315=FACE_BOUND('',#464,.T.);
#316=FACE_BOUND('',#465,.T.);
#317=FACE_BOUND('',#467,.T.);
#318=FACE_BOUND('',#468,.T.);
#319=FACE_BOUND('',#469,.T.);
#320=FACE_BOUND('',#482,.T.);
#321=FACE_BOUND('',#484,.T.);
#322=FACE_BOUND('',#486,.T.);
#323=FACE_BOUND('',#488,.T.);
#324=FACE_BOUND('',#490,.T.);
#325=FACE_BOUND('',#492,.T.);
#326=FACE_BOUND('',#506,.T.);
#327=FACE_BOUND('',#508,.T.);
#328=B_SPLINE_CURVE_WITH_KNOTS('',3,(#1923,#1924,#1925,#1926,#1927,#1928,
#1929,#1930,#1931,#1932,#1933,#1934,#1935,#1936,#1937,#1938,#1939,#1940,
#1941,#1942,#1943,#1944,#1945),.UNSPECIFIED.,.F.,.F.,(4,2,2,2,2,3,2,2,2,
2,4),(-0.44021020401708,-0.36937623196026,-0.276548406644596,-0.183720581328932,
-0.0918602906644662,0.,0.0918602906644663,0.183720581328932,0.276548406644596,
0.36937623196026,0.440210204017081),.UNSPECIFIED.);
#329=B_SPLINE_CURVE_WITH_KNOTS('',3,(#1949,#1950,#1951,#1952,#1953,#1954,
#1955,#1956,#1957,#1958,#1959,#1960,#1961,#1962,#1963,#1964,#1965,#1966,
#1967,#1968,#1969,#1970,#1971),.UNSPECIFIED.,.F.,.F.,(4,2,2,2,2,3,2,2,2,
2,4),(2.57327484364004,2.64410881569686,2.73693664101252,2.82976446632818,
2.92162475699265,3.01348504765712,3.10534533832158,3.19720562898605,3.29003345430171,
3.38286127961738,3.4536952516742),.UNSPECIFIED.);
#330=B_SPLINE_CURVE_WITH_KNOTS('',3,(#2206,#2207,#2208,#2209,#2210,#2211,
#2212,#2213,#2214,#2215,#2216,#2217,#2218,#2219,#2220,#2221,#2222,#2223,
#2224,#2225,#2226,#2227,#2228,#2229,#2230,#2231,#2232,#2233,#2234,#2235,
#2236,#2237,#2238,#2239,#2240,#2241),.UNSPECIFIED.,.F.,.F.,(4,2,2,2,2,2,
2,2,2,2,2,2,2,2,2,2,2,4),(-2.10359968512681,-2.08103107378187,-1.94554547637383,
-1.81489062645829,-1.67930255990407,-1.54858519329573,-1.4128945990498,
-1.28211064575253,-1.14631742275592,-1.01546315460342,-0.879567162984071,
-0.748639172872498,-0.612640237993188,-0.481635418621005,-0.345533335297706,
-0.214448857835685,-0.107555631958328,-1.00000006098E-6),.UNSPECIFIED.);
#331=B_SPLINE_CURVE_WITH_KNOTS('',3,(#2244,#2245,#2246,#2247,#2248,#2249,
#2250,#2251,#2252,#2253,#2254,#2255,#2256,#2257,#2258,#2259,#2260,#2261,
#2262,#2263,#2264,#2265,#2266,#2267,#2268,#2269,#2270,#2271,#2272,#2273,
#2274,#2275,#2276,#2277,#2278,#2279),.UNSPECIFIED.,.F.,.F.,(4,2,2,2,2,2,
2,2,2,2,2,2,2,2,2,2,2,4),(-7.85905825298031,-7.77422257041908,-7.68856054816734,
-7.55762981443557,-7.42483713253212,-7.29377710370425,-7.16107861802676,
-7.02988205164815,-6.89727499829573,-6.76593520312556,-6.63341646303585,
-6.50192733294177,-6.36949343700113,-6.23784947539028,-6.10549661518781,
-5.97369294985523,-5.84141699375484,-5.75028258696816),.UNSPECIFIED.);
#332=B_SPLINE_CURVE_WITH_KNOTS('',3,(#2284,#2285,#2286,#2287,#2288,#2289,
#2290,#2291,#2292,#2293,#2294,#2295,#2296,#2297,#2298,#2299,#2300,#2301,
#2302,#2303,#2304,#2305,#2306,#2307,#2308,#2309,#2310,#2311,#2312,#2313,
#2314,#2315,#2316,#2317,#2318,#2319),.UNSPECIFIED.,.F.,.F.,(4,2,2,2,2,2,
2,2,2,2,2,2,2,2,2,2,2,4),(-4.24214101358173,-4.2048914410257,-4.0725209662614,
-3.93981233390169,-3.80504628747379,-3.67468269995894,-3.53981327635047,
-3.40942661287122,-3.27445407429178,-3.14403745333268,-3.00896202440863,
-2.87850898785149,-2.74333084956052,-2.61283536277767,-2.47755464868551,
-2.34701109546997,-2.21162788996109,-2.10359968512681),.UNSPECIFIED.);
#333=B_SPLINE_CURVE_WITH_KNOTS('',3,(#2320,#2321,#2322,#2323,#2324,#2325,
#2326,#2327,#2328,#2329,#2330,#2331,#2332,#2333,#2334,#2335,#2336,#2337,
#2338,#2339,#2340,#2341,#2342,#2343,#2344,#2345,#2346,#2347,#2348,#2349,
#2350,#2351,#2352,#2353,#2354,#2355),.UNSPECIFIED.,.F.,.F.,(4,2,2,2,2,2,
2,2,2,2,2,2,2,2,2,2,2,4),(-5.75028258696816,-5.70944938231978,-5.5772458963651,
-5.44511072272886,-5.31297499576572,-5.18066925825091,-5.04859633055591,
-4.91611762256936,-4.78410231721224,-4.65144880140821,-4.51948575755063,
-4.38665613455588,-4.25473984189617,-4.12173331469736,-3.9869206349123,
-3.85673226776102,-3.72181712106248,-3.61699531260759),.UNSPECIFIED.);
#334=B_SPLINE_CURVE_WITH_KNOTS('',3,(#2361,#2362,#2363,#2364,#2365,#2366,
#2367,#2368,#2369,#2370,#2371,#2372,#2373,#2374,#2375,#2376,#2377,#2378,
#2379,#2380,#2381,#2382,#2383,#2384,#2385,#2386),.UNSPECIFIED.,.F.,.F.,
(4,2,2,2,2,2,2,2,2,2,2,2,4),(-1.47913833354922,-1.46458034294253,-1.32874299195507,
-1.19791685147926,-1.06197629089818,-0.931067644878991,-0.795023617953509,
-0.664030178278347,-0.527882410827952,-0.396802102620113,-0.260550306708762,
-0.129381249781886,0.),.UNSPECIFIED.);
#335=B_SPLINE_CURVE_WITH_KNOTS('',3,(#2389,#2390,#2391,#2392,#2393,#2394,
#2395,#2396,#2397,#2398,#2399,#2400,#2401,#2402,#2403,#2404,#2405,#2406,
#2407,#2408,#2409,#2410,#2411,#2412,#2413,#2414),.UNSPECIFIED.,.F.,.F.,
(4,2,2,2,2,2,2,2,2,2,2,2,4),(-7.86794629923482,-7.75493027201567,-7.64410086775257,
-7.51059875662567,-7.37975989227452,-7.24636016292494,-7.11541902959003,
-6.98212034736466,-6.85106811014228,-6.71786884131222,-6.58669715245899,
-6.45359533086519,-6.3781872802266),.UNSPECIFIED.);
#336=B_SPLINE_CURVE_WITH_KNOTS('',3,(#2434,#2435,#2436,#2437,#2438,#2439,
#2440,#2441,#2442,#2443),.UNSPECIFIED.,.F.,.F.,(4,2,2,2,4),(-0.0148421019360754,
-0.00739951306522483,-0.00292666249453577,-0.00127970164740186,-9.99986987752639E-7),
 .UNSPECIFIED.);
#337=B_SPLINE_CURVE_WITH_KNOTS('',3,(#2445,#2446,#2447,#2448,#2449,#2450),
 .UNSPECIFIED.,.F.,.F.,(4,2,4),(-0.180846840101061,-0.090528276541627,0.),
 .UNSPECIFIED.);
#338=B_SPLINE_CURVE_WITH_KNOTS('',3,(#2463,#2464,#2465,#2466,#2467,#2468,
#2469,#2470,#2471,#2472),.UNSPECIFIED.,.F.,.F.,(4,2,2,2,4),(-0.0149535669506096,
-0.00745287259980322,-0.00294348211124755,-0.00128449704857332,-9.9998565003534E-7),
 .UNSPECIFIED.);
#339=B_SPLINE_CURVE_WITH_KNOTS('',3,(#2474,#2475,#2476,#2477,#2478,#2479),
 .UNSPECIFIED.,.F.,.F.,(4,2,4),(-0.175510513051521,-0.0877546644588136,
0.),.UNSPECIFIED.);
#340=B_SPLINE_CURVE_WITH_KNOTS('',3,(#2482,#2483,#2484,#2485,#2486,#2487,
#2488,#2489,#2490,#2491,#2492,#2493,#2494,#2495,#2496,#2497,#2498,#2499,
#2500,#2501,#2502,#2503,#2504,#2505,#2506,#2507,#2508,#2509,#2510,#2511,
#2512,#2513,#2514,#2515,#2516,#2517,#2518,#2519),.UNSPECIFIED.,.F.,.F.,
(4,2,2,2,2,2,2,2,2,2,2,2,2,2,2,2,2,2,4),(-2.13108149573488,-1.98745320394869,
-1.82962548528831,-1.75200556231172,-1.60034896227162,-1.52279658772495,
-1.44711497528505,-1.29911129776284,-1.22404068635087,-1.08179010710472,
-1.0085761418628,-0.861083913552298,-0.717667486586238,-0.573740353327516,
-0.434041348236743,-0.293705087973695,-0.157727772352155,-0.077033910772711,
-9.99999999695689E-7),.UNSPECIFIED.);
#341=B_SPLINE_CURVE_WITH_KNOTS('',3,(#2520,#2521,#2522,#2523,#2524,#2525,
#2526),.UNSPECIFIED.,.F.,.F.,(4,3,4),(7.22896027101832E-5,0.000673496122850043,
0.000922700028579017),.UNSPECIFIED.);
#342=B_SPLINE_CURVE_WITH_KNOTS('',3,(#2528,#2529,#2530,#2531,#2532,#2533,
#2534,#2535,#2536,#2537,#2538,#2539,#2540,#2541,#2542,#2543,#2544,#2545,
#2546,#2547,#2548,#2549,#2550,#2551,#2552,#2553,#2554,#2555,#2556,#2557,
#2558,#2559,#2560,#2561,#2562,#2563,#2564,#2565),.UNSPECIFIED.,.F.,.F.,
(4,2,2,2,2,2,2,2,2,2,2,2,2,2,2,2,2,2,4),(-2.29340180701325,-2.11049201367315,
-1.93667869438381,-1.74180997494295,-1.56431695471365,-1.39962964819881,
-1.32507267661721,-1.18000971802147,-1.10543583249726,-0.962600865033504,
-0.814892434644476,-0.675985071317851,-0.531921231285643,-0.396796501805424,
-0.327537591697273,-0.257520735009541,-0.126772402545597,-0.0643607479537848,
0.),.UNSPECIFIED.);
#343=B_SPLINE_CURVE_WITH_KNOTS('',3,(#2566,#2567,#2568,#2569,#2570,#2571,
#2572),.UNSPECIFIED.,.F.,.F.,(4,3,4),(7.245944684394E-5,0.000594859777658842,
0.000926310213851899),.UNSPECIFIED.);
#344=B_SPLINE_CURVE_WITH_KNOTS('',3,(#2626,#2627,#2628,#2629,#2630,#2631,
#2632,#2633,#2634,#2635,#2636,#2637,#2638,#2639,#2640,#2641,#2642,#2643,
#2644,#2645,#2646,#2647,#2648,#2649,#2650,#2651,#2652,#2653,#2654,#2655,
#2656,#2657,#2658,#2659,#2660,#2661),.UNSPECIFIED.,.F.,.F.,(4,2,2,2,2,2,
2,2,2,2,2,2,2,2,2,2,2,4),(-6.3781872802266,-6.32229624691882,-6.18928947170399,
-6.05785556861833,-5.92494126266469,-5.79336572062519,-5.66054086162208,
-5.52881738788514,-5.39607860064442,-5.26420150715983,-5.13154507277188,
-4.99950929385351,-4.86693116428519,-4.73473226477145,-4.60222808246359,
-4.46986225672851,-4.33742737861098,-4.24214101358173),.UNSPECIFIED.);
#345=B_SPLINE_CURVE_WITH_KNOTS('',3,(#2662,#2663,#2664,#2665,#2666,#2667,
#2668,#2669,#2670,#2671,#2672,#2673,#2674,#2675,#2676,#2677,#2678,#2679,
#2680,#2681,#2682,#2683,#2684,#2685,#2686,#2687,#2688,#2689,#2690,#2691,
#2692,#2693,#2694,#2695,#2696,#2697),.UNSPECIFIED.,.F.,.F.,(4,2,2,2,2,2,
2,2,2,2,2,2,2,2,2,2,2,4),(-3.61699531260759,-3.59158532582943,-3.45656783651849,
-3.32628708491561,-3.19116732808102,-3.06083249774886,-2.92561049944977,
-2.79521686028228,-2.6598925990378,-2.52943579674619,-2.39400920604108,
-2.26348524364329,-2.12795621518432,-1.99736143304626,-1.86172982053373,
-1.73106087551919,-1.59532649873018,-1.47913833354922),.UNSPECIFIED.);
#346=FACE_OUTER_BOUND('',#422,.T.);
#347=FACE_OUTER_BOUND('',#424,.T.);
#348=FACE_OUTER_BOUND('',#425,.T.);
#349=FACE_OUTER_BOUND('',#426,.T.);
#350=FACE_OUTER_BOUND('',#427,.T.);
#351=FACE_OUTER_BOUND('',#428,.T.);
#352=FACE_OUTER_BOUND('',#429,.T.);
#353=FACE_OUTER_BOUND('',#430,.T.);
#354=FACE_OUTER_BOUND('',#431,.T.);
#355=FACE_OUTER_BOUND('',#432,.T.);
#356=FACE_OUTER_BOUND('',#433,.T.);
#357=FACE_OUTER_BOUND('',#434,.T.);
#358=FACE_OUTER_BOUND('',#435,.T.);
#359=FACE_OUTER_BOUND('',#436,.T.);
#360=FACE_OUTER_BOUND('',#437,.T.);
#361=FACE_OUTER_BOUND('',#439,.T.);
#362=FACE_OUTER_BOUND('',#441,.T.);
#363=FACE_OUTER_BOUND('',#443,.T.);
#364=FACE_OUTER_BOUND('',#445,.T.);
#365=FACE_OUTER_BOUND('',#446,.T.);
#366=FACE_OUTER_BOUND('',#447,.T.);
#367=FACE_OUTER_BOUND('',#448,.T.);
#368=FACE_OUTER_BOUND('',#449,.T.);
#369=FACE_OUTER_BOUND('',#450,.T.);
#370=FACE_OUTER_BOUND('',#451,.T.);
#371=FACE_OUTER_BOUND('',#452,.T.);
#372=FACE_OUTER_BOUND('',#453,.T.);
#373=FACE_OUTER_BOUND('',#454,.T.);
#374=FACE_OUTER_BOUND('',#455,.T.);
#375=FACE_OUTER_BOUND('',#456,.T.);
#376=FACE_OUTER_BOUND('',#457,.T.);
#377=FACE_OUTER_BOUND('',#458,.T.);
#378=FACE_OUTER_BOUND('',#459,.T.);
#379=FACE_OUTER_BOUND('',#460,.T.);
#380=FACE_OUTER_BOUND('',#461,.T.);
#381=FACE_OUTER_BOUND('',#462,.T.);
#382=FACE_OUTER_BOUND('',#466,.T.);
#383=FACE_OUTER_BOUND('',#470,.T.);
#384=FACE_OUTER_BOUND('',#471,.T.);
#385=FACE_OUTER_BOUND('',#472,.T.);
#386=FACE_OUTER_BOUND('',#473,.T.);
#387=FACE_OUTER_BOUND('',#474,.T.);
#388=FACE_OUTER_BOUND('',#475,.T.);
#389=FACE_OUTER_BOUND('',#476,.T.);
#390=FACE_OUTER_BOUND('',#477,.T.);
#391=FACE_OUTER_BOUND('',#478,.T.);
#392=FACE_OUTER_BOUND('',#479,.T.);
#393=FACE_OUTER_BOUND('',#480,.T.);
#394=FACE_OUTER_BOUND('',#481,.T.);
#395=FACE_OUTER_BOUND('',#483,.T.);
#396=FACE_OUTER_BOUND('',#485,.T.);
#397=FACE_OUTER_BOUND('',#487,.T.);
#398=FACE_OUTER_BOUND('',#489,.T.);
#399=FACE_OUTER_BOUND('',#491,.T.);
#400=FACE_OUTER_BOUND('',#493,.T.);
#401=FACE_OUTER_BOUND('',#494,.T.);
#402=FACE_OUTER_BOUND('',#495,.T.);
#403=FACE_OUTER_BOUND('',#496,.T.);
#404=FACE_OUTER_BOUND('',#497,.T.);
#405=FACE_OUTER_BOUND('',#498,.T.);
#406=FACE_OUTER_BOUND('',#499,.T.);
#407=FACE_OUTER_BOUND('',#500,.T.);
#408=FACE_OUTER_BOUND('',#501,.T.);
#409=FACE_OUTER_BOUND('',#502,.T.);
#410=FACE_OUTER_BOUND('',#503,.T.);
#411=FACE_OUTER_BOUND('',#504,.T.);
#412=FACE_OUTER_BOUND('',#505,.T.);
#413=FACE_OUTER_BOUND('',#507,.T.);
#414=FACE_OUTER_BOUND('',#509,.T.);
#415=FACE_OUTER_BOUND('',#510,.T.);
#416=FACE_OUTER_BOUND('',#511,.T.);
#417=FACE_OUTER_BOUND('',#512,.T.);
#418=FACE_OUTER_BOUND('',#513,.T.);
#419=FACE_OUTER_BOUND('',#514,.T.);
#420=FACE_OUTER_BOUND('',#515,.T.);
#421=FACE_OUTER_BOUND('',#516,.T.);
#422=EDGE_LOOP('',(#861,#862,#863,#864));
#423=EDGE_LOOP('',(#865,#866,#867,#868));
#424=EDGE_LOOP('',(#869,#870,#871,#872,#873,#874));
#425=EDGE_LOOP('',(#875,#876,#877,#878));
#426=EDGE_LOOP('',(#879,#880,#881,#882,#883));
#427=EDGE_LOOP('',(#884,#885,#886,#887));
#428=EDGE_LOOP('',(#888,#889,#890,#891,#892));
#429=EDGE_LOOP('',(#893,#894,#895,#896));
#430=EDGE_LOOP('',(#897,#898,#899,#900,#901));
#431=EDGE_LOOP('',(#902));
#432=EDGE_LOOP('',(#903,#904,#905,#906));
#433=EDGE_LOOP('',(#907,#908,#909,#910));
#434=EDGE_LOOP('',(#911,#912,#913,#914));
#435=EDGE_LOOP('',(#915,#916,#917,#918));
#436=EDGE_LOOP('',(#919,#920,#921,#922));
#437=EDGE_LOOP('',(#923,#924,#925,#926));
#438=EDGE_LOOP('',(#927));
#439=EDGE_LOOP('',(#928,#929,#930,#931));
#440=EDGE_LOOP('',(#932));
#441=EDGE_LOOP('',(#933,#934,#935,#936,#937,#938));
#442=EDGE_LOOP('',(#939));
#443=EDGE_LOOP('',(#940,#941,#942,#943,#944,#945));
#444=EDGE_LOOP('',(#946));
#445=EDGE_LOOP('',(#947,#948,#949,#950));
#446=EDGE_LOOP('',(#951,#952,#953,#954));
#447=EDGE_LOOP('',(#955,#956,#957,#958));
#448=EDGE_LOOP('',(#959,#960,#961,#962));
#449=EDGE_LOOP('',(#963));
#450=EDGE_LOOP('',(#964));
#451=EDGE_LOOP('',(#965,#966,#967,#968));
#452=EDGE_LOOP('',(#969,#970,#971,#972,#973,#974));
#453=EDGE_LOOP('',(#975,#976,#977,#978,#979));
#454=EDGE_LOOP('',(#980,#981,#982,#983,#984));
#455=EDGE_LOOP('',(#985,#986,#987,#988));
#456=EDGE_LOOP('',(#989));
#457=EDGE_LOOP('',(#990));
#458=EDGE_LOOP('',(#991,#992,#993,#994));
#459=EDGE_LOOP('',(#995,#996,#997,#998));
#460=EDGE_LOOP('',(#999,#1000,#1001,#1002));
#461=EDGE_LOOP('',(#1003,#1004,#1005,#1006));
#462=EDGE_LOOP('',(#1007,#1008,#1009,#1010,#1011,#1012));
#463=EDGE_LOOP('',(#1013));
#464=EDGE_LOOP('',(#1014));
#465=EDGE_LOOP('',(#1015));
#466=EDGE_LOOP('',(#1016,#1017,#1018,#1019,#1020,#1021));
#467=EDGE_LOOP('',(#1022));
#468=EDGE_LOOP('',(#1023));
#469=EDGE_LOOP('',(#1024));
#470=EDGE_LOOP('',(#1025,#1026,#1027,#1028));
#471=EDGE_LOOP('',(#1029,#1030,#1031,#1032));
#472=EDGE_LOOP('',(#1033,#1034,#1035,#1036));
#473=EDGE_LOOP('',(#1037,#1038,#1039,#1040));
#474=EDGE_LOOP('',(#1041,#1042,#1043,#1044));
#475=EDGE_LOOP('',(#1045,#1046,#1047,#1048));
#476=EDGE_LOOP('',(#1049,#1050,#1051,#1052));
#477=EDGE_LOOP('',(#1053,#1054,#1055,#1056));
#478=EDGE_LOOP('',(#1057,#1058,#1059,#1060));
#479=EDGE_LOOP('',(#1061,#1062,#1063,#1064));
#480=EDGE_LOOP('',(#1065,#1066,#1067,#1068));
#481=EDGE_LOOP('',(#1069));
#482=EDGE_LOOP('',(#1070));
#483=EDGE_LOOP('',(#1071));
#484=EDGE_LOOP('',(#1072));
#485=EDGE_LOOP('',(#1073));
#486=EDGE_LOOP('',(#1074));
#487=EDGE_LOOP('',(#1075));
#488=EDGE_LOOP('',(#1076));
#489=EDGE_LOOP('',(#1077));
#490=EDGE_LOOP('',(#1078));
#491=EDGE_LOOP('',(#1079));
#492=EDGE_LOOP('',(#1080));
#493=EDGE_LOOP('',(#1081,#1082,#1083,#1084));
#494=EDGE_LOOP('',(#1085,#1086,#1087,#1088));
#495=EDGE_LOOP('',(#1089,#1090,#1091,#1092));
#496=EDGE_LOOP('',(#1093,#1094,#1095,#1096,#1097));
#497=EDGE_LOOP('',(#1098,#1099,#1100,#1101));
#498=EDGE_LOOP('',(#1102,#1103,#1104,#1105,#1106,#1107,#1108));
#499=EDGE_LOOP('',(#1109,#1110,#1111,#1112,#1113,#1114,#1115));
#500=EDGE_LOOP('',(#1116,#1117,#1118,#1119,#1120));
#501=EDGE_LOOP('',(#1121,#1122,#1123,#1124,#1125));
#502=EDGE_LOOP('',(#1126,#1127,#1128,#1129,#1130,#1131,#1132,#1133,#1134));
#503=EDGE_LOOP('',(#1135,#1136,#1137,#1138,#1139,#1140,#1141,#1142,#1143,
#1144));
#504=EDGE_LOOP('',(#1145,#1146,#1147,#1148));
#505=EDGE_LOOP('',(#1149));
#506=EDGE_LOOP('',(#1150));
#507=EDGE_LOOP('',(#1151));
#508=EDGE_LOOP('',(#1152));
#509=EDGE_LOOP('',(#1153,#1154,#1155,#1156));
#510=EDGE_LOOP('',(#1157,#1158,#1159,#1160));
#511=EDGE_LOOP('',(#1161,#1162,#1163,#1164));
#512=EDGE_LOOP('',(#1165,#1166,#1167,#1168));
#513=EDGE_LOOP('',(#1169,#1170,#1171,#1172));
#514=EDGE_LOOP('',(#1173,#1174,#1175,#1176));
#515=EDGE_LOOP('',(#1177,#1178,#1179,#1180,#1181,#1182,#1183,#1184,#1185));
#516=EDGE_LOOP('',(#1186,#1187,#1188,#1189,#1190,#1191,#1192,#1193,#1194));
#517=CIRCLE('',#1356,5.);
#518=CIRCLE('',#1357,15.);
#519=CIRCLE('',#1358,23.);
#520=CIRCLE('',#1359,23.);
#521=CIRCLE('',#1361,4.);
#522=CIRCLE('',#1362,4.);
#523=CIRCLE('',#1363,4.);
#524=CIRCLE('',#1364,4.);
#525=CIRCLE('',#1374,4.5);
#526=CIRCLE('',#1375,0.5);
#527=CIRCLE('',#1376,4.);
#528=CIRCLE('',#1378,4.5);
#529=CIRCLE('',#1379,0.5);
#530=CIRCLE('',#1380,4.);
#531=CIRCLE('',#1382,4.);
#532=CIRCLE('',#1384,4.);
#533=CIRCLE('',#1386,4.5);
#534=CIRCLE('',#1387,4.5);
#535=CIRCLE('',#1400,4.5);
#536=CIRCLE('',#1401,0.5);
#537=CIRCLE('',#1402,4.);
#538=CIRCLE('',#1404,4.5);
#539=CIRCLE('',#1405,0.5);
#540=CIRCLE('',#1406,4.);
#541=CIRCLE('',#1407,4.);
#542=CIRCLE('',#1408,4.5);
#543=CIRCLE('',#1410,4.);
#544=CIRCLE('',#1413,4.);
#545=CIRCLE('',#1418,4.);
#546=CIRCLE('',#1419,4.);
#547=CIRCLE('',#1421,4.);
#548=CIRCLE('',#1422,4.);
#549=CIRCLE('',#1424,4.);
#550=CIRCLE('',#1425,4.);
#551=CIRCLE('',#1427,10.);
#552=CIRCLE('',#1428,10.);
#553=CIRCLE('',#1430,9.99999951505478);
#554=CIRCLE('',#1431,10.);
#555=CIRCLE('',#1433,10.);
#556=CIRCLE('',#1434,9.99999951505478);
#557=CIRCLE('',#1442,8.);
#558=CIRCLE('',#1443,8.);
#559=CIRCLE('',#1445,20.);
#560=CIRCLE('',#1446,20.);
#561=CIRCLE('',#1448,17.);
#562=CIRCLE('',#1449,17.);
#563=CIRCLE('',#1451,20.);
#564=CIRCLE('',#1452,20.);
#565=CIRCLE('',#1454,8.);
#566=CIRCLE('',#1455,8.);
#567=CIRCLE('',#1457,4.5);
#568=CIRCLE('',#1458,4.5);
#569=CIRCLE('',#1467,3.4);
#570=CIRCLE('',#1470,3.4);
#571=CIRCLE('',#1472,5.5021444402588);
#572=CIRCLE('',#1473,0.5);
#573=CIRCLE('',#1474,5.73919435177631);
#574=CIRCLE('',#1475,5.73919435177631);
#575=CIRCLE('',#1477,5.73919435177631);
#576=CIRCLE('',#1478,0.5);
#577=CIRCLE('',#1479,5.5021444402588);
#578=CIRCLE('',#1481,3.95355339059327);
#579=CIRCLE('',#1482,3.95355339059327);
#580=CIRCLE('',#1483,0.5);
#581=CIRCLE('',#1484,4.30710678118655);
#582=CIRCLE('',#1486,4.30710678118655);
#583=CIRCLE('',#1487,0.5);
#584=CIRCLE('',#1488,3.95355339059327);
#585=CIRCLE('',#1489,3.95355339059327);
#586=VERTEX_POINT('',#1918);
#587=VERTEX_POINT('',#1921);
#588=VERTEX_POINT('',#1922);
#589=VERTEX_POINT('',#1946);
#590=VERTEX_POINT('',#1948);
#591=VERTEX_POINT('',#1974);
#592=VERTEX_POINT('',#1975);
#593=VERTEX_POINT('',#1977);
#594=VERTEX_POINT('',#1979);
#595=VERTEX_POINT('',#1984);
#596=VERTEX_POINT('',#1986);
#597=VERTEX_POINT('',#1990);
#598=VERTEX_POINT('',#1992);
#599=VERTEX_POINT('',#2006);
#600=VERTEX_POINT('',#2008);
#601=VERTEX_POINT('',#2012);
#602=VERTEX_POINT('',#2014);
#603=VERTEX_POINT('',#2018);
#604=VERTEX_POINT('',#2022);
#605=VERTEX_POINT('',#2026);
#606=VERTEX_POINT('',#2028);
#607=VERTEX_POINT('',#2032);
#608=VERTEX_POINT('',#2033);
#609=VERTEX_POINT('',#2035);
#610=VERTEX_POINT('',#2037);
#611=VERTEX_POINT('',#2041);
#612=VERTEX_POINT('',#2042);
#613=VERTEX_POINT('',#2044);
#614=VERTEX_POINT('',#2046);
#615=VERTEX_POINT('',#2050);
#616=VERTEX_POINT('',#2053);
#617=VERTEX_POINT('',#2057);
#618=VERTEX_POINT('',#2059);
#619=VERTEX_POINT('',#2073);
#620=VERTEX_POINT('',#2075);
#621=VERTEX_POINT('',#2079);
#622=VERTEX_POINT('',#2080);
#623=VERTEX_POINT('',#2082);
#624=VERTEX_POINT('',#2084);
#625=VERTEX_POINT('',#2089);
#626=VERTEX_POINT('',#2095);
#627=VERTEX_POINT('',#2102);
#628=VERTEX_POINT('',#2104);
#629=VERTEX_POINT('',#2108);
#630=VERTEX_POINT('',#2110);
#631=VERTEX_POINT('',#2114);
#632=VERTEX_POINT('',#2116);
#633=VERTEX_POINT('',#2120);
#634=VERTEX_POINT('',#2121);
#635=VERTEX_POINT('',#2123);
#636=VERTEX_POINT('',#2125);
#637=VERTEX_POINT('',#2129);
#638=VERTEX_POINT('',#2131);
#639=VERTEX_POINT('',#2133);
#640=VERTEX_POINT('',#2135);
#641=VERTEX_POINT('',#2139);
#642=VERTEX_POINT('',#2141);
#643=VERTEX_POINT('',#2143);
#644=VERTEX_POINT('',#2145);
#645=VERTEX_POINT('',#2159);
#646=VERTEX_POINT('',#2161);
#647=VERTEX_POINT('',#2165);
#648=VERTEX_POINT('',#2167);
#649=VERTEX_POINT('',#2171);
#650=VERTEX_POINT('',#2173);
#651=VERTEX_POINT('',#2177);
#652=VERTEX_POINT('',#2179);
#653=VERTEX_POINT('',#2183);
#654=VERTEX_POINT('',#2185);
#655=VERTEX_POINT('',#2189);
#656=VERTEX_POINT('',#2191);
#657=VERTEX_POINT('',#2202);
#658=VERTEX_POINT('',#2203);
#659=VERTEX_POINT('',#2205);
#660=VERTEX_POINT('',#2242);
#661=VERTEX_POINT('',#2281);
#662=VERTEX_POINT('',#2282);
#663=VERTEX_POINT('',#2357);
#664=VERTEX_POINT('',#2358);
#665=VERTEX_POINT('',#2360);
#666=VERTEX_POINT('',#2387);
#667=VERTEX_POINT('',#2416);
#668=VERTEX_POINT('',#2418);
#669=VERTEX_POINT('',#2420);
#670=VERTEX_POINT('',#2424);
#671=VERTEX_POINT('',#2426);
#672=VERTEX_POINT('',#2430);
#673=VERTEX_POINT('',#2431);
#674=VERTEX_POINT('',#2433);
#675=VERTEX_POINT('',#2444);
#676=VERTEX_POINT('',#2452);
#677=VERTEX_POINT('',#2456);
#678=VERTEX_POINT('',#2458);
#679=VERTEX_POINT('',#2460);
#680=VERTEX_POINT('',#2462);
#681=VERTEX_POINT('',#2473);
#682=VERTEX_POINT('',#2574);
#683=VERTEX_POINT('',#2575);
#684=VERTEX_POINT('',#2579);
#685=VERTEX_POINT('',#2583);
#686=VERTEX_POINT('',#2588);
#687=VERTEX_POINT('',#2592);
#688=VERTEX_POINT('',#2600);
#689=VERTEX_POINT('',#2601);
#690=VERTEX_POINT('',#2605);
#691=VERTEX_POINT('',#2609);
#692=VERTEX_POINT('',#2614);
#693=VERTEX_POINT('',#2618);
#694=EDGE_CURVE('',#586,#586,#517,.T.);
#695=EDGE_CURVE('',#586,#586,#518,.T.);
#696=EDGE_CURVE('',#587,#588,#328,.T.);
#697=EDGE_CURVE('',#589,#587,#519,.T.);
#698=EDGE_CURVE('',#590,#589,#329,.F.);
#699=EDGE_CURVE('',#588,#590,#520,.T.);
#700=EDGE_CURVE('',#591,#592,#521,.T.);
#701=EDGE_CURVE('',#592,#593,#522,.T.);
#702=EDGE_CURVE('',#593,#594,#152,.T.);
#703=EDGE_CURVE('',#594,#594,#523,.T.);
#704=EDGE_CURVE('',#593,#591,#524,.T.);
#705=EDGE_CURVE('',#595,#591,#153,.T.);
#706=EDGE_CURVE('',#596,#595,#154,.T.);
#707=EDGE_CURVE('',#592,#596,#155,.T.);
#708=EDGE_CURVE('',#597,#592,#156,.T.);
#709=EDGE_CURVE('',#598,#597,#157,.T.);
#710=EDGE_CURVE('',#591,#598,#158,.T.);
#711=EDGE_CURVE('',#590,#595,#159,.T.);
#712=EDGE_CURVE('',#589,#596,#160,.T.);
#713=EDGE_CURVE('',#588,#598,#161,.T.);
#714=EDGE_CURVE('',#587,#597,#162,.T.);
#715=EDGE_CURVE('',#599,#599,#525,.T.);
#716=EDGE_CURVE('',#599,#600,#526,.T.);
#717=EDGE_CURVE('',#600,#600,#527,.T.);
#718=EDGE_CURVE('',#601,#601,#528,.T.);
#719=EDGE_CURVE('',#601,#602,#529,.T.);
#720=EDGE_CURVE('',#602,#602,#530,.T.);
#721=EDGE_CURVE('',#600,#603,#163,.T.);
#722=EDGE_CURVE('',#603,#603,#531,.T.);
#723=EDGE_CURVE('',#602,#604,#164,.T.);
#724=EDGE_CURVE('',#604,#604,#532,.T.);
#725=EDGE_CURVE('',#605,#605,#533,.T.);
#726=EDGE_CURVE('',#605,#606,#165,.T.);
#727=EDGE_CURVE('',#606,#606,#534,.T.);
#728=EDGE_CURVE('',#607,#608,#166,.T.);
#729=EDGE_CURVE('',#609,#608,#167,.T.);
#730=EDGE_CURVE('',#610,#609,#168,.T.);
#731=EDGE_CURVE('',#610,#607,#169,.T.);
#732=EDGE_CURVE('',#611,#612,#170,.T.);
#733=EDGE_CURVE('',#613,#612,#171,.T.);
#734=EDGE_CURVE('',#614,#613,#172,.T.);
#735=EDGE_CURVE('',#614,#611,#173,.T.);
#736=EDGE_CURVE('',#609,#615,#174,.T.);
#737=EDGE_CURVE('',#615,#614,#175,.T.);
#738=EDGE_CURVE('',#613,#616,#176,.T.);
#739=EDGE_CURVE('',#616,#610,#177,.T.);
#740=EDGE_CURVE('',#608,#617,#178,.T.);
#741=EDGE_CURVE('',#618,#607,#179,.T.);
#742=EDGE_CURVE('',#612,#618,#180,.T.);
#743=EDGE_CURVE('',#617,#611,#181,.T.);
#744=EDGE_CURVE('',#615,#617,#182,.T.);
#745=EDGE_CURVE('',#616,#618,#183,.T.);
#746=EDGE_CURVE('',#619,#619,#535,.T.);
#747=EDGE_CURVE('',#619,#620,#536,.T.);
#748=EDGE_CURVE('',#620,#620,#537,.T.);
#749=EDGE_CURVE('',#621,#622,#538,.T.);
#750=EDGE_CURVE('',#622,#623,#539,.T.);
#751=EDGE_CURVE('',#624,#623,#540,.T.);
#752=EDGE_CURVE('',#623,#624,#541,.T.);
#753=EDGE_CURVE('',#622,#621,#542,.T.);
#754=EDGE_CURVE('',#625,#625,#543,.T.);
#755=EDGE_CURVE('',#625,#624,#184,.T.);
#756=EDGE_CURVE('',#621,#619,#185,.T.);
#757=EDGE_CURVE('',#620,#626,#186,.T.);
#758=EDGE_CURVE('',#626,#626,#544,.T.);
#759=EDGE_CURVE('',#627,#627,#545,.T.);
#760=EDGE_CURVE('',#627,#628,#187,.T.);
#761=EDGE_CURVE('',#628,#628,#546,.T.);
#762=EDGE_CURVE('',#629,#629,#547,.T.);
#763=EDGE_CURVE('',#629,#630,#188,.T.);
#764=EDGE_CURVE('',#630,#630,#548,.T.);
#765=EDGE_CURVE('',#631,#631,#549,.T.);
#766=EDGE_CURVE('',#631,#632,#189,.T.);
#767=EDGE_CURVE('',#632,#632,#550,.T.);
#768=EDGE_CURVE('',#633,#634,#551,.T.);
#769=EDGE_CURVE('',#633,#635,#190,.T.);
#770=EDGE_CURVE('',#635,#636,#552,.T.);
#771=EDGE_CURVE('',#634,#636,#191,.T.);
#772=EDGE_CURVE('',#634,#637,#192,.T.);
#773=EDGE_CURVE('',#637,#638,#553,.T.);
#774=EDGE_CURVE('',#638,#639,#193,.T.);
#775=EDGE_CURVE('',#639,#640,#554,.T.);
#776=EDGE_CURVE('',#640,#633,#194,.T.);
#777=EDGE_CURVE('',#641,#635,#195,.T.);
#778=EDGE_CURVE('',#642,#641,#555,.T.);
#779=EDGE_CURVE('',#643,#642,#196,.T.);
#780=EDGE_CURVE('',#644,#643,#556,.T.);
#781=EDGE_CURVE('',#636,#644,#197,.T.);
#782=EDGE_CURVE('',#637,#644,#198,.T.);
#783=EDGE_CURVE('',#638,#643,#199,.T.);
#784=EDGE_CURVE('',#639,#642,#200,.T.);
#785=EDGE_CURVE('',#640,#641,#201,.T.);
#786=EDGE_CURVE('',#645,#645,#557,.T.);
#787=EDGE_CURVE('',#645,#646,#202,.T.);
#788=EDGE_CURVE('',#646,#646,#558,.T.);
#789=EDGE_CURVE('',#647,#647,#559,.T.);
#790=EDGE_CURVE('',#647,#648,#203,.T.);
#791=EDGE_CURVE('',#648,#648,#560,.T.);
#792=EDGE_CURVE('',#649,#649,#561,.T.);
#793=EDGE_CURVE('',#649,#650,#204,.T.);
#794=EDGE_CURVE('',#650,#650,#562,.T.);
#795=EDGE_CURVE('',#651,#651,#563,.T.);
#796=EDGE_CURVE('',#651,#652,#205,.T.);
#797=EDGE_CURVE('',#652,#652,#564,.T.);
#798=EDGE_CURVE('',#653,#653,#565,.T.);
#799=EDGE_CURVE('',#653,#654,#206,.T.);
#800=EDGE_CURVE('',#654,#654,#566,.T.);
#801=EDGE_CURVE('',#655,#655,#567,.T.);
#802=EDGE_CURVE('',#655,#656,#207,.T.);
#803=EDGE_CURVE('',#656,#656,#568,.T.);
#804=EDGE_CURVE('',#657,#658,#208,.T.);
#805=EDGE_CURVE('',#658,#659,#330,.T.);
#806=EDGE_CURVE('',#659,#660,#569,.T.);
#807=EDGE_CURVE('',#657,#660,#331,.F.);
#808=EDGE_CURVE('',#661,#662,#209,.T.);
#809=EDGE_CURVE('',#662,#658,#332,.T.);
#810=EDGE_CURVE('',#661,#657,#333,.F.);
#811=EDGE_CURVE('',#663,#664,#210,.T.);
#812=EDGE_CURVE('',#665,#663,#334,.F.);
#813=EDGE_CURVE('',#665,#666,#570,.T.);
#814=EDGE_CURVE('',#666,#664,#335,.T.);
#815=EDGE_CURVE('',#667,#667,#571,.T.);
#816=EDGE_CURVE('',#667,#668,#572,.T.);
#817=EDGE_CURVE('',#669,#668,#573,.T.);
#818=EDGE_CURVE('',#668,#669,#574,.T.);
#819=EDGE_CURVE('',#670,#670,#575,.T.);
#820=EDGE_CURVE('',#670,#671,#576,.T.);
#821=EDGE_CURVE('',#671,#671,#577,.T.);
#822=EDGE_CURVE('',#672,#673,#578,.T.);
#823=EDGE_CURVE('',#674,#672,#336,.T.);
#824=EDGE_CURVE('',#675,#674,#337,.T.);
#825=EDGE_CURVE('',#673,#675,#579,.T.);
#826=EDGE_CURVE('',#673,#676,#580,.T.);
#827=EDGE_CURVE('',#676,#676,#581,.T.);
#828=EDGE_CURVE('',#677,#677,#582,.T.);
#829=EDGE_CURVE('',#677,#678,#583,.T.);
#830=EDGE_CURVE('',#679,#678,#584,.T.);
#831=EDGE_CURVE('',#680,#679,#338,.T.);
#832=EDGE_CURVE('',#681,#680,#339,.T.);
#833=EDGE_CURVE('',#678,#681,#585,.T.);
#834=EDGE_CURVE('',#666,#675,#340,.F.);
#835=EDGE_CURVE('',#672,#665,#341,.T.);
#836=EDGE_CURVE('',#660,#681,#342,.F.);
#837=EDGE_CURVE('',#679,#659,#343,.T.);
#838=EDGE_CURVE('',#682,#683,#73,.T.);
#839=EDGE_CURVE('',#684,#682,#74,.T.);
#840=EDGE_CURVE('',#685,#684,#75,.T.);
#841=EDGE_CURVE('',#685,#670,#211,.T.);
#842=EDGE_CURVE('',#686,#685,#76,.T.);
#843=EDGE_CURVE('',#687,#686,#77,.T.);
#844=EDGE_CURVE('',#683,#687,#78,.T.);
#845=EDGE_CURVE('',#688,#689,#79,.T.);
#846=EDGE_CURVE('',#690,#688,#80,.T.);
#847=EDGE_CURVE('',#691,#690,#81,.T.);
#848=EDGE_CURVE('',#691,#669,#212,.T.);
#849=EDGE_CURVE('',#692,#691,#82,.T.);
#850=EDGE_CURVE('',#693,#692,#83,.T.);
#851=EDGE_CURVE('',#689,#693,#84,.T.);
#852=EDGE_CURVE('',#664,#662,#344,.T.);
#853=EDGE_CURVE('',#663,#661,#345,.F.);
#854=EDGE_CURVE('',#690,#682,#213,.T.);
#855=EDGE_CURVE('',#691,#683,#214,.T.);
#856=EDGE_CURVE('',#692,#687,#215,.T.);
#857=EDGE_CURVE('',#693,#686,#216,.T.);
#858=EDGE_CURVE('',#689,#685,#217,.T.);
#859=EDGE_CURVE('',#688,#684,#218,.T.);
#860=EDGE_CURVE('',#674,#680,#85,.T.);
#861=ORIENTED_EDGE('',*,*,#694,.F.);
#862=ORIENTED_EDGE('',*,*,#695,.T.);
#863=ORIENTED_EDGE('',*,*,#694,.T.);
#864=ORIENTED_EDGE('',*,*,#695,.F.);
#865=ORIENTED_EDGE('',*,*,#696,.F.);
#866=ORIENTED_EDGE('',*,*,#697,.F.);
#867=ORIENTED_EDGE('',*,*,#698,.F.);
#868=ORIENTED_EDGE('',*,*,#699,.F.);
#869=ORIENTED_EDGE('',*,*,#700,.T.);
#870=ORIENTED_EDGE('',*,*,#701,.T.);
#871=ORIENTED_EDGE('',*,*,#702,.T.);
#872=ORIENTED_EDGE('',*,*,#703,.F.);
#873=ORIENTED_EDGE('',*,*,#702,.F.);
#874=ORIENTED_EDGE('',*,*,#704,.T.);
#875=ORIENTED_EDGE('',*,*,#700,.F.);
#876=ORIENTED_EDGE('',*,*,#705,.F.);
#877=ORIENTED_EDGE('',*,*,#706,.F.);
#878=ORIENTED_EDGE('',*,*,#707,.F.);
#879=ORIENTED_EDGE('',*,*,#701,.F.);
#880=ORIENTED_EDGE('',*,*,#708,.F.);
#881=ORIENTED_EDGE('',*,*,#709,.F.);
#882=ORIENTED_EDGE('',*,*,#710,.F.);
#883=ORIENTED_EDGE('',*,*,#704,.F.);
#884=ORIENTED_EDGE('',*,*,#711,.F.);
#885=ORIENTED_EDGE('',*,*,#698,.T.);
#886=ORIENTED_EDGE('',*,*,#712,.T.);
#887=ORIENTED_EDGE('',*,*,#706,.T.);
#888=ORIENTED_EDGE('',*,*,#713,.F.);
#889=ORIENTED_EDGE('',*,*,#699,.T.);
#890=ORIENTED_EDGE('',*,*,#711,.T.);
#891=ORIENTED_EDGE('',*,*,#705,.T.);
#892=ORIENTED_EDGE('',*,*,#710,.T.);
#893=ORIENTED_EDGE('',*,*,#714,.F.);
#894=ORIENTED_EDGE('',*,*,#696,.T.);
#895=ORIENTED_EDGE('',*,*,#713,.T.);
#896=ORIENTED_EDGE('',*,*,#709,.T.);
#897=ORIENTED_EDGE('',*,*,#712,.F.);
#898=ORIENTED_EDGE('',*,*,#697,.T.);
#899=ORIENTED_EDGE('',*,*,#714,.T.);
#900=ORIENTED_EDGE('',*,*,#708,.T.);
#901=ORIENTED_EDGE('',*,*,#707,.T.);
#902=ORIENTED_EDGE('',*,*,#703,.T.);
#903=ORIENTED_EDGE('',*,*,#715,.F.);
#904=ORIENTED_EDGE('',*,*,#716,.T.);
#905=ORIENTED_EDGE('',*,*,#717,.F.);
#906=ORIENTED_EDGE('',*,*,#716,.F.);
#907=ORIENTED_EDGE('',*,*,#718,.F.);
#908=ORIENTED_EDGE('',*,*,#719,.T.);
#909=ORIENTED_EDGE('',*,*,#720,.F.);
#910=ORIENTED_EDGE('',*,*,#719,.F.);
#911=ORIENTED_EDGE('',*,*,#717,.T.);
#912=ORIENTED_EDGE('',*,*,#721,.T.);
#913=ORIENTED_EDGE('',*,*,#722,.F.);
#914=ORIENTED_EDGE('',*,*,#721,.F.);
#915=ORIENTED_EDGE('',*,*,#720,.T.);
#916=ORIENTED_EDGE('',*,*,#723,.T.);
#917=ORIENTED_EDGE('',*,*,#724,.F.);
#918=ORIENTED_EDGE('',*,*,#723,.F.);
#919=ORIENTED_EDGE('',*,*,#725,.T.);
#920=ORIENTED_EDGE('',*,*,#726,.T.);
#921=ORIENTED_EDGE('',*,*,#727,.F.);
#922=ORIENTED_EDGE('',*,*,#726,.F.);
#923=ORIENTED_EDGE('',*,*,#728,.T.);
#924=ORIENTED_EDGE('',*,*,#729,.F.);
#925=ORIENTED_EDGE('',*,*,#730,.F.);
#926=ORIENTED_EDGE('',*,*,#731,.T.);
#927=ORIENTED_EDGE('',*,*,#715,.T.);
#928=ORIENTED_EDGE('',*,*,#732,.T.);
#929=ORIENTED_EDGE('',*,*,#733,.F.);
#930=ORIENTED_EDGE('',*,*,#734,.F.);
#931=ORIENTED_EDGE('',*,*,#735,.T.);
#932=ORIENTED_EDGE('',*,*,#718,.T.);
#933=ORIENTED_EDGE('',*,*,#736,.T.);
#934=ORIENTED_EDGE('',*,*,#737,.T.);
#935=ORIENTED_EDGE('',*,*,#734,.T.);
#936=ORIENTED_EDGE('',*,*,#738,.T.);
#937=ORIENTED_EDGE('',*,*,#739,.T.);
#938=ORIENTED_EDGE('',*,*,#730,.T.);
#939=ORIENTED_EDGE('',*,*,#725,.F.);
#940=ORIENTED_EDGE('',*,*,#740,.F.);
#941=ORIENTED_EDGE('',*,*,#728,.F.);
#942=ORIENTED_EDGE('',*,*,#741,.F.);
#943=ORIENTED_EDGE('',*,*,#742,.F.);
#944=ORIENTED_EDGE('',*,*,#732,.F.);
#945=ORIENTED_EDGE('',*,*,#743,.F.);
#946=ORIENTED_EDGE('',*,*,#727,.T.);
#947=ORIENTED_EDGE('',*,*,#740,.T.);
#948=ORIENTED_EDGE('',*,*,#744,.F.);
#949=ORIENTED_EDGE('',*,*,#736,.F.);
#950=ORIENTED_EDGE('',*,*,#729,.T.);
#951=ORIENTED_EDGE('',*,*,#743,.T.);
#952=ORIENTED_EDGE('',*,*,#735,.F.);
#953=ORIENTED_EDGE('',*,*,#737,.F.);
#954=ORIENTED_EDGE('',*,*,#744,.T.);
#955=ORIENTED_EDGE('',*,*,#742,.T.);
#956=ORIENTED_EDGE('',*,*,#745,.F.);
#957=ORIENTED_EDGE('',*,*,#738,.F.);
#958=ORIENTED_EDGE('',*,*,#733,.T.);
#959=ORIENTED_EDGE('',*,*,#741,.T.);
#960=ORIENTED_EDGE('',*,*,#731,.F.);
#961=ORIENTED_EDGE('',*,*,#739,.F.);
#962=ORIENTED_EDGE('',*,*,#745,.T.);
#963=ORIENTED_EDGE('',*,*,#724,.T.);
#964=ORIENTED_EDGE('',*,*,#722,.T.);
#965=ORIENTED_EDGE('',*,*,#746,.F.);
#966=ORIENTED_EDGE('',*,*,#747,.T.);
#967=ORIENTED_EDGE('',*,*,#748,.F.);
#968=ORIENTED_EDGE('',*,*,#747,.F.);
#969=ORIENTED_EDGE('',*,*,#749,.T.);
#970=ORIENTED_EDGE('',*,*,#750,.T.);
#971=ORIENTED_EDGE('',*,*,#751,.F.);
#972=ORIENTED_EDGE('',*,*,#752,.F.);
#973=ORIENTED_EDGE('',*,*,#750,.F.);
#974=ORIENTED_EDGE('',*,*,#753,.T.);
#975=ORIENTED_EDGE('',*,*,#754,.F.);
#976=ORIENTED_EDGE('',*,*,#755,.T.);
#977=ORIENTED_EDGE('',*,*,#751,.T.);
#978=ORIENTED_EDGE('',*,*,#752,.T.);
#979=ORIENTED_EDGE('',*,*,#755,.F.);
#980=ORIENTED_EDGE('',*,*,#749,.F.);
#981=ORIENTED_EDGE('',*,*,#756,.T.);
#982=ORIENTED_EDGE('',*,*,#746,.T.);
#983=ORIENTED_EDGE('',*,*,#756,.F.);
#984=ORIENTED_EDGE('',*,*,#753,.F.);
#985=ORIENTED_EDGE('',*,*,#748,.T.);
#986=ORIENTED_EDGE('',*,*,#757,.T.);
#987=ORIENTED_EDGE('',*,*,#758,.T.);
#988=ORIENTED_EDGE('',*,*,#757,.F.);
#989=ORIENTED_EDGE('',*,*,#758,.F.);
#990=ORIENTED_EDGE('',*,*,#754,.T.);
#991=ORIENTED_EDGE('',*,*,#759,.T.);
#992=ORIENTED_EDGE('',*,*,#760,.T.);
#993=ORIENTED_EDGE('',*,*,#761,.F.);
#994=ORIENTED_EDGE('',*,*,#760,.F.);
#995=ORIENTED_EDGE('',*,*,#762,.T.);
#996=ORIENTED_EDGE('',*,*,#763,.T.);
#997=ORIENTED_EDGE('',*,*,#764,.F.);
#998=ORIENTED_EDGE('',*,*,#763,.F.);
#999=ORIENTED_EDGE('',*,*,#765,.T.);
#1000=ORIENTED_EDGE('',*,*,#766,.T.);
#1001=ORIENTED_EDGE('',*,*,#767,.F.);
#1002=ORIENTED_EDGE('',*,*,#766,.F.);
#1003=ORIENTED_EDGE('',*,*,#768,.F.);
#1004=ORIENTED_EDGE('',*,*,#769,.T.);
#1005=ORIENTED_EDGE('',*,*,#770,.T.);
#1006=ORIENTED_EDGE('',*,*,#771,.F.);
#1007=ORIENTED_EDGE('',*,*,#768,.T.);
#1008=ORIENTED_EDGE('',*,*,#772,.T.);
#1009=ORIENTED_EDGE('',*,*,#773,.T.);
#1010=ORIENTED_EDGE('',*,*,#774,.T.);
#1011=ORIENTED_EDGE('',*,*,#775,.T.);
#1012=ORIENTED_EDGE('',*,*,#776,.T.);
#1013=ORIENTED_EDGE('',*,*,#765,.F.);
#1014=ORIENTED_EDGE('',*,*,#759,.F.);
#1015=ORIENTED_EDGE('',*,*,#762,.F.);
#1016=ORIENTED_EDGE('',*,*,#770,.F.);
#1017=ORIENTED_EDGE('',*,*,#777,.F.);
#1018=ORIENTED_EDGE('',*,*,#778,.F.);
#1019=ORIENTED_EDGE('',*,*,#779,.F.);
#1020=ORIENTED_EDGE('',*,*,#780,.F.);
#1021=ORIENTED_EDGE('',*,*,#781,.F.);
#1022=ORIENTED_EDGE('',*,*,#767,.T.);
#1023=ORIENTED_EDGE('',*,*,#761,.T.);
#1024=ORIENTED_EDGE('',*,*,#764,.T.);
#1025=ORIENTED_EDGE('',*,*,#781,.T.);
#1026=ORIENTED_EDGE('',*,*,#782,.F.);
#1027=ORIENTED_EDGE('',*,*,#772,.F.);
#1028=ORIENTED_EDGE('',*,*,#771,.T.);
#1029=ORIENTED_EDGE('',*,*,#780,.T.);
#1030=ORIENTED_EDGE('',*,*,#783,.F.);
#1031=ORIENTED_EDGE('',*,*,#773,.F.);
#1032=ORIENTED_EDGE('',*,*,#782,.T.);
#1033=ORIENTED_EDGE('',*,*,#779,.T.);
#1034=ORIENTED_EDGE('',*,*,#784,.F.);
#1035=ORIENTED_EDGE('',*,*,#774,.F.);
#1036=ORIENTED_EDGE('',*,*,#783,.T.);
#1037=ORIENTED_EDGE('',*,*,#778,.T.);
#1038=ORIENTED_EDGE('',*,*,#785,.F.);
#1039=ORIENTED_EDGE('',*,*,#775,.F.);
#1040=ORIENTED_EDGE('',*,*,#784,.T.);
#1041=ORIENTED_EDGE('',*,*,#777,.T.);
#1042=ORIENTED_EDGE('',*,*,#769,.F.);
#1043=ORIENTED_EDGE('',*,*,#776,.F.);
#1044=ORIENTED_EDGE('',*,*,#785,.T.);
#1045=ORIENTED_EDGE('',*,*,#786,.F.);
#1046=ORIENTED_EDGE('',*,*,#787,.T.);
#1047=ORIENTED_EDGE('',*,*,#788,.T.);
#1048=ORIENTED_EDGE('',*,*,#787,.F.);
#1049=ORIENTED_EDGE('',*,*,#789,.F.);
#1050=ORIENTED_EDGE('',*,*,#790,.T.);
#1051=ORIENTED_EDGE('',*,*,#791,.T.);
#1052=ORIENTED_EDGE('',*,*,#790,.F.);
#1053=ORIENTED_EDGE('',*,*,#792,.F.);
#1054=ORIENTED_EDGE('',*,*,#793,.T.);
#1055=ORIENTED_EDGE('',*,*,#794,.T.);
#1056=ORIENTED_EDGE('',*,*,#793,.F.);
#1057=ORIENTED_EDGE('',*,*,#795,.F.);
#1058=ORIENTED_EDGE('',*,*,#796,.T.);
#1059=ORIENTED_EDGE('',*,*,#797,.T.);
#1060=ORIENTED_EDGE('',*,*,#796,.F.);
#1061=ORIENTED_EDGE('',*,*,#798,.F.);
#1062=ORIENTED_EDGE('',*,*,#799,.T.);
#1063=ORIENTED_EDGE('',*,*,#800,.T.);
#1064=ORIENTED_EDGE('',*,*,#799,.F.);
#1065=ORIENTED_EDGE('',*,*,#801,.F.);
#1066=ORIENTED_EDGE('',*,*,#802,.T.);
#1067=ORIENTED_EDGE('',*,*,#803,.T.);
#1068=ORIENTED_EDGE('',*,*,#802,.F.);
#1069=ORIENTED_EDGE('',*,*,#798,.T.);
#1070=ORIENTED_EDGE('',*,*,#803,.F.);
#1071=ORIENTED_EDGE('',*,*,#795,.T.);
#1072=ORIENTED_EDGE('',*,*,#800,.F.);
#1073=ORIENTED_EDGE('',*,*,#797,.F.);
#1074=ORIENTED_EDGE('',*,*,#792,.T.);
#1075=ORIENTED_EDGE('',*,*,#789,.T.);
#1076=ORIENTED_EDGE('',*,*,#794,.F.);
#1077=ORIENTED_EDGE('',*,*,#791,.F.);
#1078=ORIENTED_EDGE('',*,*,#786,.T.);
#1079=ORIENTED_EDGE('',*,*,#788,.F.);
#1080=ORIENTED_EDGE('',*,*,#801,.T.);
#1081=ORIENTED_EDGE('',*,*,#804,.T.);
#1082=ORIENTED_EDGE('',*,*,#805,.T.);
#1083=ORIENTED_EDGE('',*,*,#806,.T.);
#1084=ORIENTED_EDGE('',*,*,#807,.F.);
#1085=ORIENTED_EDGE('',*,*,#808,.T.);
#1086=ORIENTED_EDGE('',*,*,#809,.T.);
#1087=ORIENTED_EDGE('',*,*,#804,.F.);
#1088=ORIENTED_EDGE('',*,*,#810,.F.);
#1089=ORIENTED_EDGE('',*,*,#811,.F.);
#1090=ORIENTED_EDGE('',*,*,#812,.F.);
#1091=ORIENTED_EDGE('',*,*,#813,.T.);
#1092=ORIENTED_EDGE('',*,*,#814,.T.);
#1093=ORIENTED_EDGE('',*,*,#815,.F.);
#1094=ORIENTED_EDGE('',*,*,#816,.T.);
#1095=ORIENTED_EDGE('',*,*,#817,.F.);
#1096=ORIENTED_EDGE('',*,*,#818,.F.);
#1097=ORIENTED_EDGE('',*,*,#816,.F.);
#1098=ORIENTED_EDGE('',*,*,#819,.F.);
#1099=ORIENTED_EDGE('',*,*,#820,.T.);
#1100=ORIENTED_EDGE('',*,*,#821,.F.);
#1101=ORIENTED_EDGE('',*,*,#820,.F.);
#1102=ORIENTED_EDGE('',*,*,#822,.F.);
#1103=ORIENTED_EDGE('',*,*,#823,.F.);
#1104=ORIENTED_EDGE('',*,*,#824,.F.);
#1105=ORIENTED_EDGE('',*,*,#825,.F.);
#1106=ORIENTED_EDGE('',*,*,#826,.T.);
#1107=ORIENTED_EDGE('',*,*,#827,.F.);
#1108=ORIENTED_EDGE('',*,*,#826,.F.);
#1109=ORIENTED_EDGE('',*,*,#828,.F.);
#1110=ORIENTED_EDGE('',*,*,#829,.T.);
#1111=ORIENTED_EDGE('',*,*,#830,.F.);
#1112=ORIENTED_EDGE('',*,*,#831,.F.);
#1113=ORIENTED_EDGE('',*,*,#832,.F.);
#1114=ORIENTED_EDGE('',*,*,#833,.F.);
#1115=ORIENTED_EDGE('',*,*,#829,.F.);
#1116=ORIENTED_EDGE('',*,*,#834,.F.);
#1117=ORIENTED_EDGE('',*,*,#813,.F.);
#1118=ORIENTED_EDGE('',*,*,#835,.F.);
#1119=ORIENTED_EDGE('',*,*,#822,.T.);
#1120=ORIENTED_EDGE('',*,*,#825,.T.);
#1121=ORIENTED_EDGE('',*,*,#836,.F.);
#1122=ORIENTED_EDGE('',*,*,#806,.F.);
#1123=ORIENTED_EDGE('',*,*,#837,.F.);
#1124=ORIENTED_EDGE('',*,*,#830,.T.);
#1125=ORIENTED_EDGE('',*,*,#833,.T.);
#1126=ORIENTED_EDGE('',*,*,#838,.F.);
#1127=ORIENTED_EDGE('',*,*,#839,.F.);
#1128=ORIENTED_EDGE('',*,*,#840,.F.);
#1129=ORIENTED_EDGE('',*,*,#841,.T.);
#1130=ORIENTED_EDGE('',*,*,#819,.T.);
#1131=ORIENTED_EDGE('',*,*,#841,.F.);
#1132=ORIENTED_EDGE('',*,*,#842,.F.);
#1133=ORIENTED_EDGE('',*,*,#843,.F.);
#1134=ORIENTED_EDGE('',*,*,#844,.F.);
#1135=ORIENTED_EDGE('',*,*,#845,.F.);
#1136=ORIENTED_EDGE('',*,*,#846,.F.);
#1137=ORIENTED_EDGE('',*,*,#847,.F.);
#1138=ORIENTED_EDGE('',*,*,#848,.T.);
#1139=ORIENTED_EDGE('',*,*,#817,.T.);
#1140=ORIENTED_EDGE('',*,*,#818,.T.);
#1141=ORIENTED_EDGE('',*,*,#848,.F.);
#1142=ORIENTED_EDGE('',*,*,#849,.F.);
#1143=ORIENTED_EDGE('',*,*,#850,.F.);
#1144=ORIENTED_EDGE('',*,*,#851,.F.);
#1145=ORIENTED_EDGE('',*,*,#811,.T.);
#1146=ORIENTED_EDGE('',*,*,#852,.T.);
#1147=ORIENTED_EDGE('',*,*,#808,.F.);
#1148=ORIENTED_EDGE('',*,*,#853,.F.);
#1149=ORIENTED_EDGE('',*,*,#815,.T.);
#1150=ORIENTED_EDGE('',*,*,#827,.T.);
#1151=ORIENTED_EDGE('',*,*,#821,.T.);
#1152=ORIENTED_EDGE('',*,*,#828,.T.);
#1153=ORIENTED_EDGE('',*,*,#854,.T.);
#1154=ORIENTED_EDGE('',*,*,#838,.T.);
#1155=ORIENTED_EDGE('',*,*,#855,.F.);
#1156=ORIENTED_EDGE('',*,*,#847,.T.);
#1157=ORIENTED_EDGE('',*,*,#855,.T.);
#1158=ORIENTED_EDGE('',*,*,#844,.T.);
#1159=ORIENTED_EDGE('',*,*,#856,.F.);
#1160=ORIENTED_EDGE('',*,*,#849,.T.);
#1161=ORIENTED_EDGE('',*,*,#856,.T.);
#1162=ORIENTED_EDGE('',*,*,#843,.T.);
#1163=ORIENTED_EDGE('',*,*,#857,.F.);
#1164=ORIENTED_EDGE('',*,*,#850,.T.);
#1165=ORIENTED_EDGE('',*,*,#857,.T.);
#1166=ORIENTED_EDGE('',*,*,#842,.T.);
#1167=ORIENTED_EDGE('',*,*,#858,.F.);
#1168=ORIENTED_EDGE('',*,*,#851,.T.);
#1169=ORIENTED_EDGE('',*,*,#858,.T.);
#1170=ORIENTED_EDGE('',*,*,#840,.T.);
#1171=ORIENTED_EDGE('',*,*,#859,.F.);
#1172=ORIENTED_EDGE('',*,*,#845,.T.);
#1173=ORIENTED_EDGE('',*,*,#859,.T.);
#1174=ORIENTED_EDGE('',*,*,#839,.T.);
#1175=ORIENTED_EDGE('',*,*,#854,.F.);
#1176=ORIENTED_EDGE('',*,*,#846,.T.);
#1177=ORIENTED_EDGE('',*,*,#836,.T.);
#1178=ORIENTED_EDGE('',*,*,#832,.T.);
#1179=ORIENTED_EDGE('',*,*,#860,.F.);
#1180=ORIENTED_EDGE('',*,*,#823,.T.);
#1181=ORIENTED_EDGE('',*,*,#835,.T.);
#1182=ORIENTED_EDGE('',*,*,#812,.T.);
#1183=ORIENTED_EDGE('',*,*,#853,.T.);
#1184=ORIENTED_EDGE('',*,*,#810,.T.);
#1185=ORIENTED_EDGE('',*,*,#807,.T.);
#1186=ORIENTED_EDGE('',*,*,#860,.T.);
#1187=ORIENTED_EDGE('',*,*,#831,.T.);
#1188=ORIENTED_EDGE('',*,*,#837,.T.);
#1189=ORIENTED_EDGE('',*,*,#805,.F.);
#1190=ORIENTED_EDGE('',*,*,#809,.F.);
#1191=ORIENTED_EDGE('',*,*,#852,.F.);
#1192=ORIENTED_EDGE('',*,*,#814,.F.);
#1193=ORIENTED_EDGE('',*,*,#834,.T.);
#1194=ORIENTED_EDGE('',*,*,#824,.T.);
#1195=TOROIDAL_SURFACE('',#1355,20.,5.);
#1196=TOROIDAL_SURFACE('',#1373,4.5,0.5);
#1197=TOROIDAL_SURFACE('',#1377,4.5,0.5);
#1198=TOROIDAL_SURFACE('',#1399,4.5,0.5);
#1199=TOROIDAL_SURFACE('',#1403,4.5,0.5);
#1200=TOROIDAL_SURFACE('',#1471,5.5021444402588,0.5);
#1201=TOROIDAL_SURFACE('',#1476,5.5021444402588,0.5);
#1202=TOROIDAL_SURFACE('',#1480,4.30710678118655,0.5);
#1203=TOROIDAL_SURFACE('',#1485,4.30710678118655,0.5);
#1204=ADVANCED_FACE('',(#346,#309),#1195,.T.);
#1205=ADVANCED_FACE('',(#347),#286,.T.);
#1206=ADVANCED_FACE('',(#348),#114,.F.);
#1207=ADVANCED_FACE('',(#349),#115,.F.);
#1208=ADVANCED_FACE('',(#350),#116,.F.);
#1209=ADVANCED_FACE('',(#351),#117,.F.);
#1210=ADVANCED_FACE('',(#352),#118,.F.);
#1211=ADVANCED_FACE('',(#353),#119,.F.);
#1212=ADVANCED_FACE('',(#354),#120,.T.);
#1213=ADVANCED_FACE('',(#355),#1196,.F.);
#1214=ADVANCED_FACE('',(#356),#1197,.F.);
#1215=ADVANCED_FACE('',(#357),#287,.T.);
#1216=ADVANCED_FACE('',(#358),#288,.T.);
#1217=ADVANCED_FACE('',(#359),#289,.F.);
#1218=ADVANCED_FACE('',(#360,#310),#121,.F.);
#1219=ADVANCED_FACE('',(#361,#311),#122,.F.);
#1220=ADVANCED_FACE('',(#362,#312),#123,.T.);
#1221=ADVANCED_FACE('',(#363,#313),#124,.F.);
#1222=ADVANCED_FACE('',(#364),#125,.F.);
#1223=ADVANCED_FACE('',(#365),#126,.F.);
#1224=ADVANCED_FACE('',(#366),#127,.F.);
#1225=ADVANCED_FACE('',(#367),#128,.F.);
#1226=ADVANCED_FACE('',(#368),#129,.T.);
#1227=ADVANCED_FACE('',(#369),#130,.T.);
#1228=ADVANCED_FACE('',(#370),#1198,.F.);
#1229=ADVANCED_FACE('',(#371),#1199,.F.);
#1230=ADVANCED_FACE('',(#372),#290,.T.);
#1231=ADVANCED_FACE('',(#373),#291,.T.);
#1232=ADVANCED_FACE('',(#374),#292,.T.);
#1233=ADVANCED_FACE('',(#375),#131,.F.);
#1234=ADVANCED_FACE('',(#376),#132,.F.);
#1235=ADVANCED_FACE('',(#377),#293,.F.);
#1236=ADVANCED_FACE('',(#378),#294,.F.);
#1237=ADVANCED_FACE('',(#379),#295,.F.);
#1238=ADVANCED_FACE('',(#380),#296,.T.);
#1239=ADVANCED_FACE('',(#381,#314,#315,#316),#133,.T.);
#1240=ADVANCED_FACE('',(#382,#317,#318,#319),#134,.F.);
#1241=ADVANCED_FACE('',(#383),#135,.F.);
#1242=ADVANCED_FACE('',(#384),#297,.T.);
#1243=ADVANCED_FACE('',(#385),#136,.F.);
#1244=ADVANCED_FACE('',(#386),#298,.T.);
#1245=ADVANCED_FACE('',(#387),#137,.F.);
#1246=ADVANCED_FACE('',(#388),#299,.T.);
#1247=ADVANCED_FACE('',(#389),#300,.T.);
#1248=ADVANCED_FACE('',(#390),#301,.T.);
#1249=ADVANCED_FACE('',(#391),#302,.T.);
#1250=ADVANCED_FACE('',(#392),#303,.T.);
#1251=ADVANCED_FACE('',(#393),#304,.F.);
#1252=ADVANCED_FACE('',(#394,#320),#138,.T.);
#1253=ADVANCED_FACE('',(#395,#321),#139,.T.);
#1254=ADVANCED_FACE('',(#396,#322),#140,.T.);
#1255=ADVANCED_FACE('',(#397,#323),#141,.F.);
#1256=ADVANCED_FACE('',(#398,#324),#142,.F.);
#1257=ADVANCED_FACE('',(#399,#325),#143,.F.);
#1258=ADVANCED_FACE('',(#400),#305,.F.);
#1259=ADVANCED_FACE('',(#401),#306,.F.);
#1260=ADVANCED_FACE('',(#402),#307,.F.);
#1261=ADVANCED_FACE('',(#403),#1200,.T.);
#1262=ADVANCED_FACE('',(#404),#1201,.T.);
#1263=ADVANCED_FACE('',(#405),#1202,.T.);
#1264=ADVANCED_FACE('',(#406),#1203,.T.);
#1265=ADVANCED_FACE('',(#407),#86,.F.);
#1266=ADVANCED_FACE('',(#408),#87,.F.);
#1267=ADVANCED_FACE('',(#409),#88,.T.);
#1268=ADVANCED_FACE('',(#410),#89,.T.);
#1269=ADVANCED_FACE('',(#411),#308,.F.);
#1270=ADVANCED_FACE('',(#412,#326),#144,.T.);
#1271=ADVANCED_FACE('',(#413,#327),#145,.F.);
#1272=ADVANCED_FACE('',(#414),#146,.F.);
#1273=ADVANCED_FACE('',(#415),#147,.F.);
#1274=ADVANCED_FACE('',(#416),#148,.F.);
#1275=ADVANCED_FACE('',(#417),#149,.F.);
#1276=ADVANCED_FACE('',(#418),#150,.F.);
#1277=ADVANCED_FACE('',(#419),#151,.F.);
#1278=ADVANCED_FACE('',(#420),#71,.F.);
#1279=ADVANCED_FACE('',(#421),#72,.F.);
#1280=CLOSED_SHELL('',(#1204,#1205,#1206,#1207,#1208,#1209,#1210,#1211,
#1212));
#1281=CLOSED_SHELL('',(#1213,#1214,#1215,#1216,#1217,#1218,#1219,#1220,
#1221,#1222,#1223,#1224,#1225,#1226,#1227));
#1282=CLOSED_SHELL('',(#1228,#1229,#1230,#1231,#1232,#1233,#1234));
#1283=CLOSED_SHELL('',(#1235,#1236,#1237,#1238,#1239,#1240,#1241,#1242,
#1243,#1244,#1245));
#1284=CLOSED_SHELL('',(#1246,#1247,#1248,#1249,#1250,#1251,#1252,#1253,
#1254,#1255,#1256,#1257));
#1285=CLOSED_SHELL('',(#1258,#1259,#1260,#1261,#1262,#1263,#1264,#1265,
#1266,#1267,#1268,#1269,#1270,#1271,#1272,#1273,#1274,#1275,#1276,#1277,
#1278,#1279));
#1286=DERIVED_UNIT_ELEMENT(#1298,1.);
#1287=DERIVED_UNIT_ELEMENT(#3209,-3.);
#1288=DERIVED_UNIT_ELEMENT(#1298,1.);
#1289=DERIVED_UNIT_ELEMENT(#3209,-3.);
#1290=DERIVED_UNIT_ELEMENT(#1298,1.);
#1291=DERIVED_UNIT_ELEMENT(#3209,-3.);
#1292=DERIVED_UNIT_ELEMENT(#1298,1.);
#1293=DERIVED_UNIT_ELEMENT(#3209,-3.);
#1294=DERIVED_UNIT_ELEMENT(#1298,1.);
#1295=DERIVED_UNIT_ELEMENT(#3209,-3.);
#1296=DERIVED_UNIT_ELEMENT(#1298,1.);
#1297=DERIVED_UNIT_ELEMENT(#3209,-3.);
#1298=(
MASS_UNIT()
NAMED_UNIT(*)
SI_UNIT(.KILO.,.GRAM.)
);
#1299=DERIVED_UNIT((#1286,#1287));
#1300=DERIVED_UNIT((#1288,#1289));
#1301=DERIVED_UNIT((#1290,#1291));
#1302=DERIVED_UNIT((#1292,#1293));
#1303=DERIVED_UNIT((#1294,#1295));
#1304=DERIVED_UNIT((#1296,#1297));
#1305=MEASURE_REPRESENTATION_ITEM('density measure',
POSITIVE_RATIO_MEASURE(7850.),#1299);
#1306=MEASURE_REPRESENTATION_ITEM('density measure',
POSITIVE_RATIO_MEASURE(7850.),#1300);
#1307=MEASURE_REPRESENTATION_ITEM('density measure',
POSITIVE_RATIO_MEASURE(7850.),#1301);
#1308=MEASURE_REPRESENTATION_ITEM('density measure',
POSITIVE_RATIO_MEASURE(7850.),#1302);
#1309=MEASURE_REPRESENTATION_ITEM('density measure',
POSITIVE_RATIO_MEASURE(7850.),#1303);
#1310=MEASURE_REPRESENTATION_ITEM('density measure',
POSITIVE_RATIO_MEASURE(7850.),#1304);
#1311=PROPERTY_DEFINITION_REPRESENTATION(#1341,#1323);
#1312=PROPERTY_DEFINITION_REPRESENTATION(#1342,#1324);
#1313=PROPERTY_DEFINITION_REPRESENTATION(#1343,#1325);
#1314=PROPERTY_DEFINITION_REPRESENTATION(#1344,#1326);
#1315=PROPERTY_DEFINITION_REPRESENTATION(#1345,#1327);
#1316=PROPERTY_DEFINITION_REPRESENTATION(#1346,#1328);
#1317=PROPERTY_DEFINITION_REPRESENTATION(#1347,#1329);
#1318=PROPERTY_DEFINITION_REPRESENTATION(#1348,#1330);
#1319=PROPERTY_DEFINITION_REPRESENTATION(#1349,#1331);
#1320=PROPERTY_DEFINITION_REPRESENTATION(#1350,#1332);
#1321=PROPERTY_DEFINITION_REPRESENTATION(#1351,#1333);
#1322=PROPERTY_DEFINITION_REPRESENTATION(#1352,#1334);
#1323=REPRESENTATION('material name',(#1335),#3201);
#1324=REPRESENTATION('density',(#1305),#3201);
#1325=REPRESENTATION('material name',(#1336),#3202);
#1326=REPRESENTATION('density',(#1306),#3202);
#1327=REPRESENTATION('material name',(#1337),#3203);
#1328=REPRESENTATION('density',(#1307),#3203);
#1329=REPRESENTATION('material name',(#1338),#3204);
#1330=REPRESENTATION('density',(#1308),#3204);
#1331=REPRESENTATION('material name',(#1339),#3205);
#1332=REPRESENTATION('density',(#1309),#3205);
#1333=REPRESENTATION('material name',(#1340),#3206);
#1334=REPRESENTATION('density',(#1310),#3206);
#1335=DESCRIPTIVE_REPRESENTATION_ITEM('Steel','Steel');
#1336=DESCRIPTIVE_REPRESENTATION_ITEM('Steel','Steel');
#1337=DESCRIPTIVE_REPRESENTATION_ITEM('Steel','Steel');
#1338=DESCRIPTIVE_REPRESENTATION_ITEM('Steel','Steel');
#1339=DESCRIPTIVE_REPRESENTATION_ITEM('Steel','Steel');
#1340=DESCRIPTIVE_REPRESENTATION_ITEM('Steel','Steel');
#1341=PROPERTY_DEFINITION('material property','material name',#3250);
#1342=PROPERTY_DEFINITION('material property','density of part',#3250);
#1343=PROPERTY_DEFINITION('material property','material name',#3251);
#1344=PROPERTY_DEFINITION('material property','density of part',#3251);
#1345=PROPERTY_DEFINITION('material property','material name',#3252);
#1346=PROPERTY_DEFINITION('material property','density of part',#3252);
#1347=PROPERTY_DEFINITION('material property','material name',#3253);
#1348=PROPERTY_DEFINITION('material property','density of part',#3253);
#1349=PROPERTY_DEFINITION('material property','material name',#3254);
#1350=PROPERTY_DEFINITION('material property','density of part',#3254);
#1351=PROPERTY_DEFINITION('material property','material name',#3255);
#1352=PROPERTY_DEFINITION('material property','density of part',#3255);
#1353=AXIS2_PLACEMENT_3D('',#1915,#1518,#1519);
#1354=AXIS2_PLACEMENT_3D('',#1916,#1520,#1521);
#1355=AXIS2_PLACEMENT_3D('',#1917,#1522,#1523);
#1356=AXIS2_PLACEMENT_3D('',#1919,#1524,#1525);
#1357=AXIS2_PLACEMENT_3D('',#1920,#1526,#1527);
#1358=AXIS2_PLACEMENT_3D('',#1947,#1528,#1529);
#1359=AXIS2_PLACEMENT_3D('',#1972,#1530,#1531);
#1360=AXIS2_PLACEMENT_3D('',#1973,#1532,#1533);
#1361=AXIS2_PLACEMENT_3D('',#1976,#1534,#1535);
#1362=AXIS2_PLACEMENT_3D('',#1978,#1536,#1537);
#1363=AXIS2_PLACEMENT_3D('',#1981,#1539,#1540);
#1364=AXIS2_PLACEMENT_3D('',#1982,#1541,#1542);
#1365=AXIS2_PLACEMENT_3D('',#1983,#1543,#1544);
#1366=AXIS2_PLACEMENT_3D('',#1989,#1548,#1549);
#1367=AXIS2_PLACEMENT_3D('',#1995,#1553,#1554);
#1368=AXIS2_PLACEMENT_3D('',#1998,#1557,#1558);
#1369=AXIS2_PLACEMENT_3D('',#2000,#1560,#1561);
#1370=AXIS2_PLACEMENT_3D('',#2002,#1563,#1564);
#1371=AXIS2_PLACEMENT_3D('',#2003,#1565,#1566);
#1372=AXIS2_PLACEMENT_3D('',#2004,#1567,#1568);
#1373=AXIS2_PLACEMENT_3D('',#2005,#1569,#1570);
#1374=AXIS2_PLACEMENT_3D('',#2007,#1571,#1572);
#1375=AXIS2_PLACEMENT_3D('',#2009,#1573,#1574);
#1376=AXIS2_PLACEMENT_3D('',#2010,#1575,#1576);
#1377=AXIS2_PLACEMENT_3D('',#2011,#1577,#1578);
#1378=AXIS2_PLACEMENT_3D('',#2013,#1579,#1580);
#1379=AXIS2_PLACEMENT_3D('',#2015,#1581,#1582);
#1380=AXIS2_PLACEMENT_3D('',#2016,#1583,#1584);
#1381=AXIS2_PLACEMENT_3D('',#2017,#1585,#1586);
#1382=AXIS2_PLACEMENT_3D('',#2020,#1588,#1589);
#1383=AXIS2_PLACEMENT_3D('',#2021,#1590,#1591);
#1384=AXIS2_PLACEMENT_3D('',#2024,#1593,#1594);
#1385=AXIS2_PLACEMENT_3D('',#2025,#1595,#1596);
#1386=AXIS2_PLACEMENT_3D('',#2027,#1597,#1598);
#1387=AXIS2_PLACEMENT_3D('',#2030,#1600,#1601);
#1388=AXIS2_PLACEMENT_3D('',#2031,#1602,#1603);
#1389=AXIS2_PLACEMENT_3D('',#2040,#1608,#1609);
#1390=AXIS2_PLACEMENT_3D('',#2049,#1614,#1615);
#1391=AXIS2_PLACEMENT_3D('',#2056,#1620,#1621);
#1392=AXIS2_PLACEMENT_3D('',#2063,#1626,#1627);
#1393=AXIS2_PLACEMENT_3D('',#2065,#1629,#1630);
#1394=AXIS2_PLACEMENT_3D('',#2066,#1631,#1632);
#1395=AXIS2_PLACEMENT_3D('',#2068,#1634,#1635);
#1396=AXIS2_PLACEMENT_3D('',#2069,#1636,#1637);
#1397=AXIS2_PLACEMENT_3D('',#2070,#1638,#1639);
#1398=AXIS2_PLACEMENT_3D('',#2071,#1640,#1641);
#1399=AXIS2_PLACEMENT_3D('',#2072,#1642,#1643);
#1400=AXIS2_PLACEMENT_3D('',#2074,#1644,#1645);
#1401=AXIS2_PLACEMENT_3D('',#2076,#1646,#1647);
#1402=AXIS2_PLACEMENT_3D('',#2077,#1648,#1649);
#1403=AXIS2_PLACEMENT_3D('',#2078,#1650,#1651);
#1404=AXIS2_PLACEMENT_3D('',#2081,#1652,#1653);
#1405=AXIS2_PLACEMENT_3D('',#2083,#1654,#1655);
#1406=AXIS2_PLACEMENT_3D('',#2085,#1656,#1657);
#1407=AXIS2_PLACEMENT_3D('',#2086,#1658,#1659);
#1408=AXIS2_PLACEMENT_3D('',#2087,#1660,#1661);
#1409=AXIS2_PLACEMENT_3D('',#2088,#1662,#1663);
#1410=AXIS2_PLACEMENT_3D('',#2090,#1664,#1665);
#1411=AXIS2_PLACEMENT_3D('',#2092,#1667,#1668);
#1412=AXIS2_PLACEMENT_3D('',#2094,#1670,#1671);
#1413=AXIS2_PLACEMENT_3D('',#2097,#1673,#1674);
#1414=AXIS2_PLACEMENT_3D('',#2098,#1675,#1676);
#1415=AXIS2_PLACEMENT_3D('',#2099,#1677,#1678);
#1416=AXIS2_PLACEMENT_3D('',#2100,#1679,#1680);
#1417=AXIS2_PLACEMENT_3D('',#2101,#1681,#1682);
#1418=AXIS2_PLACEMENT_3D('',#2103,#1683,#1684);
#1419=AXIS2_PLACEMENT_3D('',#2106,#1686,#1687);
#1420=AXIS2_PLACEMENT_3D('',#2107,#1688,#1689);
#1421=AXIS2_PLACEMENT_3D('',#2109,#1690,#1691);
#1422=AXIS2_PLACEMENT_3D('',#2112,#1693,#1694);
#1423=AXIS2_PLACEMENT_3D('',#2113,#1695,#1696);
#1424=AXIS2_PLACEMENT_3D('',#2115,#1697,#1698);
#1425=AXIS2_PLACEMENT_3D('',#2118,#1700,#1701);
#1426=AXIS2_PLACEMENT_3D('',#2119,#1702,#1703);
#1427=AXIS2_PLACEMENT_3D('',#2122,#1704,#1705);
#1428=AXIS2_PLACEMENT_3D('',#2126,#1707,#1708);
#1429=AXIS2_PLACEMENT_3D('',#2128,#1710,#1711);
#1430=AXIS2_PLACEMENT_3D('',#2132,#1713,#1714);
#1431=AXIS2_PLACEMENT_3D('',#2136,#1716,#1717);
#1432=AXIS2_PLACEMENT_3D('',#2138,#1719,#1720);
#1433=AXIS2_PLACEMENT_3D('',#2142,#1722,#1723);
#1434=AXIS2_PLACEMENT_3D('',#2146,#1725,#1726);
#1435=AXIS2_PLACEMENT_3D('',#2148,#1728,#1729);
#1436=AXIS2_PLACEMENT_3D('',#2150,#1731,#1732);
#1437=AXIS2_PLACEMENT_3D('',#2152,#1734,#1735);
#1438=AXIS2_PLACEMENT_3D('',#2154,#1737,#1738);
#1439=AXIS2_PLACEMENT_3D('',#2156,#1740,#1741);
#1440=AXIS2_PLACEMENT_3D('',#2157,#1742,#1743);
#1441=AXIS2_PLACEMENT_3D('',#2158,#1744,#1745);
#1442=AXIS2_PLACEMENT_3D('',#2160,#1746,#1747);
#1443=AXIS2_PLACEMENT_3D('',#2163,#1749,#1750);
#1444=AXIS2_PLACEMENT_3D('',#2164,#1751,#1752);
#1445=AXIS2_PLACEMENT_3D('',#2166,#1753,#1754);
#1446=AXIS2_PLACEMENT_3D('',#2169,#1756,#1757);
#1447=AXIS2_PLACEMENT_3D('',#2170,#1758,#1759);
#1448=AXIS2_PLACEMENT_3D('',#2172,#1760,#1761);
#1449=AXIS2_PLACEMENT_3D('',#2175,#1763,#1764);
#1450=AXIS2_PLACEMENT_3D('',#2176,#1765,#1766);
#1451=AXIS2_PLACEMENT_3D('',#2178,#1767,#1768);
#1452=AXIS2_PLACEMENT_3D('',#2181,#1770,#1771);
#1453=AXIS2_PLACEMENT_3D('',#2182,#1772,#1773);
#1454=AXIS2_PLACEMENT_3D('',#2184,#1774,#1775);
#1455=AXIS2_PLACEMENT_3D('',#2187,#1777,#1778);
#1456=AXIS2_PLACEMENT_3D('',#2188,#1779,#1780);
#1457=AXIS2_PLACEMENT_3D('',#2190,#1781,#1782);
#1458=AXIS2_PLACEMENT_3D('',#2193,#1784,#1785);
#1459=AXIS2_PLACEMENT_3D('',#2194,#1786,#1787);
#1460=AXIS2_PLACEMENT_3D('',#2195,#1788,#1789);
#1461=AXIS2_PLACEMENT_3D('',#2196,#1790,#1791);
#1462=AXIS2_PLACEMENT_3D('',#2197,#1792,#1793);
#1463=AXIS2_PLACEMENT_3D('',#2198,#1794,#1795);
#1464=AXIS2_PLACEMENT_3D('',#2199,#1796,#1797);
#1465=AXIS2_PLACEMENT_3D('',#2200,#1798,#1799);
#1466=AXIS2_PLACEMENT_3D('',#2201,#1800,#1801);
#1467=AXIS2_PLACEMENT_3D('',#2243,#1803,#1804);
#1468=AXIS2_PLACEMENT_3D('',#2280,#1805,#1806);
#1469=AXIS2_PLACEMENT_3D('',#2356,#1808,#1809);
#1470=AXIS2_PLACEMENT_3D('',#2388,#1811,#1812);
#1471=AXIS2_PLACEMENT_3D('',#2415,#1813,#1814);
#1472=AXIS2_PLACEMENT_3D('',#2417,#1815,#1816);
#1473=AXIS2_PLACEMENT_3D('',#2419,#1817,#1818);
#1474=AXIS2_PLACEMENT_3D('',#2421,#1819,#1820);
#1475=AXIS2_PLACEMENT_3D('',#2422,#1821,#1822);
#1476=AXIS2_PLACEMENT_3D('',#2423,#1823,#1824);
#1477=AXIS2_PLACEMENT_3D('',#2425,#1825,#1826);
#1478=AXIS2_PLACEMENT_3D('',#2427,#1827,#1828);
#1479=AXIS2_PLACEMENT_3D('',#2428,#1829,#1830);
#1480=AXIS2_PLACEMENT_3D('',#2429,#1831,#1832);
#1481=AXIS2_PLACEMENT_3D('',#2432,#1833,#1834);
#1482=AXIS2_PLACEMENT_3D('',#2451,#1835,#1836);
#1483=AXIS2_PLACEMENT_3D('',#2453,#1837,#1838);
#1484=AXIS2_PLACEMENT_3D('',#2454,#1839,#1840);
#1485=AXIS2_PLACEMENT_3D('',#2455,#1841,#1842);
#1486=AXIS2_PLACEMENT_3D('',#2457,#1843,#1844);
#1487=AXIS2_PLACEMENT_3D('',#2459,#1845,#1846);
#1488=AXIS2_PLACEMENT_3D('',#2461,#1847,#1848);
#1489=AXIS2_PLACEMENT_3D('',#2480,#1849,#1850);
#1490=AXIS2_PLACEMENT_3D('',#2481,#1851,#1852);
#1491=AXIS2_PLACEMENT_3D('',#2527,#1853,#1854);
#1492=AXIS2_PLACEMENT_3D('',#2573,#1855,#1856);
#1493=AXIS2_PLACEMENT_3D('',#2599,#1858,#1859);
#1494=AXIS2_PLACEMENT_3D('',#2625,#1861,#1862);
#1495=AXIS2_PLACEMENT_3D('',#2698,#1863,#1864);
#1496=AXIS2_PLACEMENT_3D('',#2699,#1865,#1866);
#1497=AXIS2_PLACEMENT_3D('',#2700,#1867,#1868);
#1498=AXIS2_PLACEMENT_3D('',#2703,#1871,#1872);
#1499=AXIS2_PLACEMENT_3D('',#2705,#1874,#1875);
#1500=AXIS2_PLACEMENT_3D('',#2707,#1877,#1878);
#1501=AXIS2_PLACEMENT_3D('',#2709,#1880,#1881);
#1502=AXIS2_PLACEMENT_3D('',#2711,#1883,#1884);
#1503=AXIS2_PLACEMENT_3D('',#3177,#1885,#1886);
#1504=AXIS2_PLACEMENT_3D('',#3178,#1887,#1888);
#1505=AXIS2_PLACEMENT_3D('',#3179,#1889,#1890);
#1506=AXIS2_PLACEMENT_3D('',#3180,#1891,#1892);
#1507=AXIS2_PLACEMENT_3D('',#3181,#1893,#1894);
#1508=AXIS2_PLACEMENT_3D('',#3182,#1895,#1896);
#1509=AXIS2_PLACEMENT_3D('',#3183,#1897,#1898);
#1510=AXIS2_PLACEMENT_3D('',#3184,#1899,#1900);
#1511=AXIS2_PLACEMENT_3D('',#3185,#1901,#1902);
#1512=AXIS2_PLACEMENT_3D('',#3186,#1903,#1904);
#1513=AXIS2_PLACEMENT_3D('',#3187,#1905,#1906);
#1514=AXIS2_PLACEMENT_3D('',#3188,#1907,#1908);
#1515=AXIS2_PLACEMENT_3D('',#3189,#1909,#1910);
#1516=AXIS2_PLACEMENT_3D('',#3190,#1911,#1912);
#1517=AXIS2_PLACEMENT_3D('',#3191,#1913,#1914);
#1518=DIRECTION('axis',(0.,0.,1.));
#1519=DIRECTION('refdir',(1.,0.,0.));
#1520=DIRECTION('axis',(0.,0.,1.));
#1521=DIRECTION('refdir',(1.,0.,0.));
#1522=DIRECTION('center_axis',(-1.73472347597681E-16,1.,0.));
#1523=DIRECTION('ref_axis',(-1.,-1.73472347597681E-16,0.));
#1524=DIRECTION('center_axis',(-1.22464679914735E-16,-2.12442355226077E-32,
-1.));
#1525=DIRECTION('ref_axis',(1.,1.73472347597681E-16,-1.22464679914735E-16));
#1526=DIRECTION('center_axis',(1.73472347597681E-16,-1.,0.));
#1527=DIRECTION('ref_axis',(-1.,-1.73472347597681E-16,0.));
#1528=DIRECTION('center_axis',(0.,1.,0.));
#1529=DIRECTION('ref_axis',(0.,0.,1.));
#1530=DIRECTION('center_axis',(0.,-1.,0.));
#1531=DIRECTION('ref_axis',(0.,0.,-1.));
#1532=DIRECTION('center_axis',(0.,0.,1.));
#1533=DIRECTION('ref_axis',(1.,0.,0.));
#1534=DIRECTION('center_axis',(0.,0.,-1.));
#1535=DIRECTION('ref_axis',(-1.,0.,0.));
#1536=DIRECTION('center_axis',(0.,0.,-1.));
#1537=DIRECTION('ref_axis',(-1.,0.,0.));
#1538=DIRECTION('',(0.,0.,-1.));
#1539=DIRECTION('center_axis',(0.,0.,-1.));
#1540=DIRECTION('ref_axis',(-1.,0.,0.));
#1541=DIRECTION('center_axis',(0.,0.,-1.));
#1542=DIRECTION('ref_axis',(-1.,0.,0.));
#1543=DIRECTION('center_axis',(0.,0.,1.));
#1544=DIRECTION('ref_axis',(1.,0.,0.));
#1545=DIRECTION('',(-1.,0.,0.));
#1546=DIRECTION('',(0.,1.,0.));
#1547=DIRECTION('',(1.,0.,0.));
#1548=DIRECTION('center_axis',(0.,0.,1.));
#1549=DIRECTION('ref_axis',(1.,0.,0.));
#1550=DIRECTION('',(1.,0.,0.));
#1551=DIRECTION('',(0.,-1.,0.));
#1552=DIRECTION('',(-1.,0.,0.));
#1553=DIRECTION('center_axis',(-1.,0.,0.));
#1554=DIRECTION('ref_axis',(0.,0.,1.));
#1555=DIRECTION('',(0.,0.,-1.));
#1556=DIRECTION('',(0.,0.,-1.));
#1557=DIRECTION('center_axis',(0.,-1.,0.));
#1558=DIRECTION('ref_axis',(0.,0.,-1.));
#1559=DIRECTION('',(0.,0.,-1.));
#1560=DIRECTION('center_axis',(1.,0.,0.));
#1561=DIRECTION('ref_axis',(0.,0.,-1.));
#1562=DIRECTION('',(0.,0.,-1.));
#1563=DIRECTION('center_axis',(0.,1.,0.));
#1564=DIRECTION('ref_axis',(0.,0.,1.));
#1565=DIRECTION('center_axis',(0.,0.,-1.));
#1566=DIRECTION('ref_axis',(-1.,0.,0.));
#1567=DIRECTION('axis',(0.,0.,1.));
#1568=DIRECTION('refdir',(1.,0.,0.));
#1569=DIRECTION('center_axis',(3.33847688608258E-16,1.,0.));
#1570=DIRECTION('ref_axis',(-1.,3.5527136788005E-16,0.));
#1571=DIRECTION('center_axis',(3.33847688608258E-16,1.,0.));
#1572=DIRECTION('ref_axis',(-1.,3.33847688608258E-16,0.));
#1573=DIRECTION('center_axis',(2.22044604925031E-16,-7.41290781221554E-32,
1.));
#1574=DIRECTION('ref_axis',(1.,-4.44089209850063E-16,-2.22044604925031E-16));
#1575=DIRECTION('center_axis',(-3.33847688608258E-16,-1.,0.));
#1576=DIRECTION('ref_axis',(-1.,3.33847688608258E-16,0.));
#1577=DIRECTION('center_axis',(1.66923844304129E-16,-1.,0.));
#1578=DIRECTION('ref_axis',(1.,0.,0.));
#1579=DIRECTION('center_axis',(1.66923844304129E-16,-1.,0.));
#1580=DIRECTION('ref_axis',(1.,1.66923844304129E-16,0.));
#1581=DIRECTION('center_axis',(-2.22044604925031E-16,-3.70645390610778E-32,
1.));
#1582=DIRECTION('ref_axis',(-1.,-2.22044604925031E-16,-2.22044604925031E-16));
#1583=DIRECTION('center_axis',(-1.66923844304129E-16,1.,0.));
#1584=DIRECTION('ref_axis',(1.,1.66923844304129E-16,0.));
#1585=DIRECTION('center_axis',(3.33847688608258E-16,1.,0.));
#1586=DIRECTION('ref_axis',(-1.,3.33847688608258E-16,0.));
#1587=DIRECTION('',(-3.33847688608258E-16,-1.,0.));
#1588=DIRECTION('center_axis',(-3.33847688608258E-16,-1.,0.));
#1589=DIRECTION('ref_axis',(1.,-3.33847688608258E-16,0.));
#1590=DIRECTION('center_axis',(1.66923844304129E-16,-1.,0.));
#1591=DIRECTION('ref_axis',(1.,1.66923844304129E-16,0.));
#1592=DIRECTION('',(-1.66923844304129E-16,1.,0.));
#1593=DIRECTION('center_axis',(-1.66923844304129E-16,1.,0.));
#1594=DIRECTION('ref_axis',(-1.,-1.66923844304129E-16,0.));
#1595=DIRECTION('center_axis',(0.,0.,-1.));
#1596=DIRECTION('ref_axis',(-1.,0.,0.));
#1597=DIRECTION('center_axis',(0.,0.,1.));
#1598=DIRECTION('ref_axis',(1.,0.,0.));
#1599=DIRECTION('',(0.,0.,-1.));
#1600=DIRECTION('center_axis',(0.,0.,1.));
#1601=DIRECTION('ref_axis',(1.,0.,0.));
#1602=DIRECTION('center_axis',(3.33847688608258E-16,1.,0.));
#1603=DIRECTION('ref_axis',(-1.,3.33847688608258E-16,0.));
#1604=DIRECTION('',(1.,-3.33847688608257E-16,0.));
#1605=DIRECTION('',(0.,0.,-1.));
#1606=DIRECTION('',(1.,-3.33847688608257E-16,0.));
#1607=DIRECTION('',(0.,0.,-1.));
#1608=DIRECTION('center_axis',(1.66923844304129E-16,-1.,0.));
#1609=DIRECTION('ref_axis',(1.,1.66923844304129E-16,0.));
#1610=DIRECTION('',(-1.,-1.66923844304129E-16,0.));
#1611=DIRECTION('',(0.,0.,-1.));
#1612=DIRECTION('',(-1.,-1.66923844304129E-16,0.));
#1613=DIRECTION('',(0.,0.,-1.));
#1614=DIRECTION('center_axis',(0.,0.,1.));
#1615=DIRECTION('ref_axis',(1.,0.,0.));
#1616=DIRECTION('',(0.499999999999999,0.866025403784439,0.));
#1617=DIRECTION('',(-0.5,0.866025403784438,0.));
#1618=DIRECTION('',(-0.5,-0.866025403784439,0.));
#1619=DIRECTION('',(0.5,-0.866025403784439,0.));
#1620=DIRECTION('center_axis',(0.,0.,1.));
#1621=DIRECTION('ref_axis',(1.,0.,0.));
#1622=DIRECTION('',(0.499999999999999,0.866025403784439,0.));
#1623=DIRECTION('',(0.5,-0.866025403784439,0.));
#1624=DIRECTION('',(-0.5,-0.866025403784439,0.));
#1625=DIRECTION('',(-0.5,0.866025403784438,0.));
#1626=DIRECTION('center_axis',(-0.866025403784439,0.5,0.));
#1627=DIRECTION('ref_axis',(-0.5,-0.866025403784439,0.));
#1628=DIRECTION('',(0.,0.,-1.));
#1629=DIRECTION('center_axis',(-0.866025403784439,-0.5,0.));
#1630=DIRECTION('ref_axis',(0.5,-0.866025403784439,0.));
#1631=DIRECTION('center_axis',(0.866025403784439,-0.5,0.));
#1632=DIRECTION('ref_axis',(0.5,0.866025403784439,0.));
#1633=DIRECTION('',(0.,0.,-1.));
#1634=DIRECTION('center_axis',(0.866025403784439,0.5,0.));
#1635=DIRECTION('ref_axis',(-0.5,0.866025403784439,0.));
#1636=DIRECTION('center_axis',(-1.66923844304129E-16,1.,0.));
#1637=DIRECTION('ref_axis',(-1.,-1.66923844304129E-16,0.));
#1638=DIRECTION('center_axis',(-3.33847688608258E-16,-1.,0.));
#1639=DIRECTION('ref_axis',(1.,-3.33847688608258E-16,0.));
#1640=DIRECTION('axis',(0.,0.,1.));
#1641=DIRECTION('refdir',(1.,0.,0.));
#1642=DIRECTION('center_axis',(-1.,0.,0.));
#1643=DIRECTION('ref_axis',(0.,0.,1.));
#1644=DIRECTION('center_axis',(-1.,0.,0.));
#1645=DIRECTION('ref_axis',(0.,0.,1.));
#1646=DIRECTION('center_axis',(0.,1.,-1.22464679914735E-16));
#1647=DIRECTION('ref_axis',(0.,-1.22464679914735E-16,-1.));
#1648=DIRECTION('center_axis',(1.,0.,0.));
#1649=DIRECTION('ref_axis',(0.,0.,1.));
#1650=DIRECTION('center_axis',(1.,0.,0.));
#1651=DIRECTION('ref_axis',(0.,0.,-1.));
#1652=DIRECTION('center_axis',(-1.,0.,0.));
#1653=DIRECTION('ref_axis',(0.,0.,1.));
#1654=DIRECTION('center_axis',(0.,1.,1.22464679914735E-16));
#1655=DIRECTION('ref_axis',(0.,-1.22464679914735E-16,1.));
#1656=DIRECTION('center_axis',(-1.,0.,0.));
#1657=DIRECTION('ref_axis',(0.,0.,-1.));
#1658=DIRECTION('center_axis',(-1.,0.,0.));
#1659=DIRECTION('ref_axis',(0.,0.,-1.));
#1660=DIRECTION('center_axis',(-1.,0.,0.));
#1661=DIRECTION('ref_axis',(0.,0.,1.));
#1662=DIRECTION('center_axis',(-1.,0.,0.));
#1663=DIRECTION('ref_axis',(0.,0.,1.));
#1664=DIRECTION('center_axis',(-1.,0.,0.));
#1665=DIRECTION('ref_axis',(0.,0.,1.));
#1666=DIRECTION('',(1.,0.,0.));
#1667=DIRECTION('center_axis',(-1.,0.,0.));
#1668=DIRECTION('ref_axis',(0.,0.,1.));
#1669=DIRECTION('',(1.,0.,0.));
#1670=DIRECTION('center_axis',(-1.,0.,0.));
#1671=DIRECTION('ref_axis',(0.,0.,1.));
#1672=DIRECTION('',(1.,0.,0.));
#1673=DIRECTION('center_axis',(-1.,0.,0.));
#1674=DIRECTION('ref_axis',(0.,0.,1.));
#1675=DIRECTION('center_axis',(-1.,0.,0.));
#1676=DIRECTION('ref_axis',(0.,0.,1.));
#1677=DIRECTION('center_axis',(1.,0.,0.));
#1678=DIRECTION('ref_axis',(0.,0.,-1.));
#1679=DIRECTION('axis',(0.,0.,1.));
#1680=DIRECTION('refdir',(1.,0.,0.));
#1681=DIRECTION('center_axis',(0.,0.,-1.));
#1682=DIRECTION('ref_axis',(-1.,0.,0.));
#1683=DIRECTION('center_axis',(0.,0.,1.));
#1684=DIRECTION('ref_axis',(1.,0.,0.));
#1685=DIRECTION('',(0.,0.,-1.));
#1686=DIRECTION('center_axis',(0.,0.,1.));
#1687=DIRECTION('ref_axis',(1.,0.,0.));
#1688=DIRECTION('center_axis',(0.,0.,-1.));
#1689=DIRECTION('ref_axis',(-1.,0.,0.));
#1690=DIRECTION('center_axis',(0.,0.,1.));
#1691=DIRECTION('ref_axis',(1.,0.,0.));
#1692=DIRECTION('',(0.,0.,-1.));
#1693=DIRECTION('center_axis',(0.,0.,1.));
#1694=DIRECTION('ref_axis',(1.,0.,0.));
#1695=DIRECTION('center_axis',(0.,0.,-1.));
#1696=DIRECTION('ref_axis',(-1.,0.,0.));
#1697=DIRECTION('center_axis',(0.,0.,1.));
#1698=DIRECTION('ref_axis',(1.,0.,0.));
#1699=DIRECTION('',(0.,0.,-1.));
#1700=DIRECTION('center_axis',(0.,0.,1.));
#1701=DIRECTION('ref_axis',(1.,0.,0.));
#1702=DIRECTION('center_axis',(0.,0.,-1.));
#1703=DIRECTION('ref_axis',(-1.,0.,0.));
#1704=DIRECTION('center_axis',(0.,0.,1.));
#1705=DIRECTION('ref_axis',(1.,0.,0.));
#1706=DIRECTION('',(0.,0.,-1.));
#1707=DIRECTION('center_axis',(0.,0.,1.));
#1708=DIRECTION('ref_axis',(1.,0.,0.));
#1709=DIRECTION('',(0.,0.,-1.));
#1710=DIRECTION('center_axis',(0.,0.,1.));
#1711=DIRECTION('ref_axis',(1.,0.,0.));
#1712=DIRECTION('',(0.478852136424395,-0.87789556978139,0.));
#1713=DIRECTION('center_axis',(0.,0.,1.));
#1714=DIRECTION('ref_axis',(1.,0.,0.));
#1715=DIRECTION('',(0.478852136424396,0.87789556978139,0.));
#1716=DIRECTION('center_axis',(0.,0.,1.));
#1717=DIRECTION('ref_axis',(1.,0.,0.));
#1718=DIRECTION('',(-1.,-1.44560289664734E-16,0.));
#1719=DIRECTION('center_axis',(0.,0.,1.));
#1720=DIRECTION('ref_axis',(1.,0.,0.));
#1721=DIRECTION('',(-1.,-1.44560289664734E-16,0.));
#1722=DIRECTION('center_axis',(0.,0.,1.));
#1723=DIRECTION('ref_axis',(1.,0.,0.));
#1724=DIRECTION('',(0.478852136424396,0.87789556978139,0.));
#1725=DIRECTION('center_axis',(0.,0.,1.));
#1726=DIRECTION('ref_axis',(1.,0.,0.));
#1727=DIRECTION('',(0.478852136424395,-0.87789556978139,0.));
#1728=DIRECTION('center_axis',(0.877895569781391,0.478852136424395,0.));
#1729=DIRECTION('ref_axis',(-0.478852136424395,0.877895569781391,0.));
#1730=DIRECTION('',(0.,0.,-1.));
#1731=DIRECTION('center_axis',(0.,0.,-1.));
#1732=DIRECTION('ref_axis',(-1.,0.,0.));
#1733=DIRECTION('',(0.,0.,-1.));
#1734=DIRECTION('center_axis',(-0.87789556978139,0.478852136424395,0.));
#1735=DIRECTION('ref_axis',(-0.478852136424395,-0.87789556978139,0.));
#1736=DIRECTION('',(0.,0.,-1.));
#1737=DIRECTION('center_axis',(0.,0.,-1.));
#1738=DIRECTION('ref_axis',(0.859898870921574,0.510464427543979,0.));
#1739=DIRECTION('',(0.,0.,-1.));
#1740=DIRECTION('center_axis',(1.44560289664734E-16,-1.,0.));
#1741=DIRECTION('ref_axis',(1.,1.44560289664734E-16,0.));
#1742=DIRECTION('axis',(0.,0.,1.));
#1743=DIRECTION('refdir',(1.,0.,0.));
#1744=DIRECTION('center_axis',(1.,0.,0.));
#1745=DIRECTION('ref_axis',(0.,0.,-1.));
#1746=DIRECTION('center_axis',(1.,0.,0.));
#1747=DIRECTION('ref_axis',(0.,0.,-1.));
#1748=DIRECTION('',(-1.,0.,0.));
#1749=DIRECTION('center_axis',(1.,0.,0.));
#1750=DIRECTION('ref_axis',(0.,0.,-1.));
#1751=DIRECTION('center_axis',(1.,0.,0.));
#1752=DIRECTION('ref_axis',(0.,0.,-1.));
#1753=DIRECTION('center_axis',(1.,0.,0.));
#1754=DIRECTION('ref_axis',(0.,0.,-1.));
#1755=DIRECTION('',(-1.,0.,0.));
#1756=DIRECTION('center_axis',(1.,0.,0.));
#1757=DIRECTION('ref_axis',(0.,0.,-1.));
#1758=DIRECTION('center_axis',(1.,0.,0.));
#1759=DIRECTION('ref_axis',(0.,0.,-1.));
#1760=DIRECTION('center_axis',(1.,0.,0.));
#1761=DIRECTION('ref_axis',(0.,0.,-1.));
#1762=DIRECTION('',(-1.,0.,0.));
#1763=DIRECTION('center_axis',(1.,0.,0.));
#1764=DIRECTION('ref_axis',(0.,0.,-1.));
#1765=DIRECTION('center_axis',(1.,0.,0.));
#1766=DIRECTION('ref_axis',(0.,0.,-1.));
#1767=DIRECTION('center_axis',(1.,0.,0.));
#1768=DIRECTION('ref_axis',(0.,0.,-1.));
#1769=DIRECTION('',(-1.,0.,0.));
#1770=DIRECTION('center_axis',(1.,0.,0.));
#1771=DIRECTION('ref_axis',(0.,0.,-1.));
#1772=DIRECTION('center_axis',(1.,0.,0.));
#1773=DIRECTION('ref_axis',(0.,0.,-1.));
#1774=DIRECTION('center_axis',(1.,0.,0.));
#1775=DIRECTION('ref_axis',(0.,0.,-1.));
#1776=DIRECTION('',(-1.,0.,0.));
#1777=DIRECTION('center_axis',(1.,0.,0.));
#1778=DIRECTION('ref_axis',(0.,0.,-1.));
#1779=DIRECTION('center_axis',(1.,0.,0.));
#1780=DIRECTION('ref_axis',(0.,0.,-1.));
#1781=DIRECTION('center_axis',(1.,0.,0.));
#1782=DIRECTION('ref_axis',(0.,0.,-1.));
#1783=DIRECTION('',(1.,0.,0.));
#1784=DIRECTION('center_axis',(1.,0.,0.));
#1785=DIRECTION('ref_axis',(0.,0.,-1.));
#1786=DIRECTION('center_axis',(1.,0.,0.));
#1787=DIRECTION('ref_axis',(0.,0.,-1.));
#1788=DIRECTION('center_axis',(1.,0.,0.));
#1789=DIRECTION('ref_axis',(0.,0.,-1.));
#1790=DIRECTION('center_axis',(-1.,0.,0.));
#1791=DIRECTION('ref_axis',(0.,0.,1.));
#1792=DIRECTION('center_axis',(-1.,0.,0.));
#1793=DIRECTION('ref_axis',(0.,0.,1.));
#1794=DIRECTION('center_axis',(1.,0.,0.));
#1795=DIRECTION('ref_axis',(0.,0.,-1.));
#1796=DIRECTION('center_axis',(1.,0.,0.));
#1797=DIRECTION('ref_axis',(0.,0.,-1.));
#1798=DIRECTION('axis',(0.,0.,1.));
#1799=DIRECTION('refdir',(1.,0.,0.));
#1800=DIRECTION('center_axis',(0.,0.,-1.));
#1801=DIRECTION('ref_axis',(-1.,0.,0.));
#1802=DIRECTION('',(0.,0.,-1.));
#1803=DIRECTION('center_axis',(0.,0.,-1.));
#1804=DIRECTION('ref_axis',(1.,-2.1316282072803E-14,0.));
#1805=DIRECTION('center_axis',(0.,0.,-1.));
#1806=DIRECTION('ref_axis',(-1.,0.,0.));
#1807=DIRECTION('',(0.,0.,-1.));
#1808=DIRECTION('center_axis',(0.,0.,-1.));
#1809=DIRECTION('ref_axis',(-1.,0.,0.));
#1810=DIRECTION('',(0.,0.,-1.));
#1811=DIRECTION('center_axis',(0.,0.,1.));
#1812=DIRECTION('ref_axis',(1.,0.,0.));
#1813=DIRECTION('center_axis',(0.,0.,1.));
#1814=DIRECTION('ref_axis',(1.,0.,0.));
#1815=DIRECTION('center_axis',(0.,0.,1.));
#1816=DIRECTION('ref_axis',(1.,0.,0.));
#1817=DIRECTION('center_axis',(1.22464679914735E-16,-1.,0.));
#1818=DIRECTION('ref_axis',(-1.,-1.22464679914735E-16,0.));
#1819=DIRECTION('center_axis',(0.,0.,-1.));
#1820=DIRECTION('ref_axis',(-1.,0.,0.));
#1821=DIRECTION('center_axis',(0.,0.,-1.));
#1822=DIRECTION('ref_axis',(-1.,0.,0.));
#1823=DIRECTION('center_axis',(0.,0.,1.));
#1824=DIRECTION('ref_axis',(1.,0.,0.));
#1825=DIRECTION('center_axis',(0.,0.,1.));
#1826=DIRECTION('ref_axis',(-1.,0.,0.));
#1827=DIRECTION('center_axis',(1.22464679914735E-16,-1.,0.));
#1828=DIRECTION('ref_axis',(-1.,-1.22464679914735E-16,0.));
#1829=DIRECTION('center_axis',(0.,0.,-1.));
#1830=DIRECTION('ref_axis',(1.,0.,0.));
#1831=DIRECTION('center_axis',(0.,0.,1.));
#1832=DIRECTION('ref_axis',(1.,0.,0.));
#1833=DIRECTION('center_axis',(0.,0.,1.));
#1834=DIRECTION('ref_axis',(-1.,0.,0.));
#1835=DIRECTION('center_axis',(0.,0.,1.));
#1836=DIRECTION('ref_axis',(-1.,0.,0.));
#1837=DIRECTION('center_axis',(1.22464679914735E-16,-1.,0.));
#1838=DIRECTION('ref_axis',(-1.,-1.22464679914735E-16,0.));
#1839=DIRECTION('center_axis',(0.,0.,-1.));
#1840=DIRECTION('ref_axis',(1.,0.,0.));
#1841=DIRECTION('center_axis',(0.,0.,1.));
#1842=DIRECTION('ref_axis',(1.,0.,0.));
#1843=DIRECTION('center_axis',(0.,0.,1.));
#1844=DIRECTION('ref_axis',(1.,0.,0.));
#1845=DIRECTION('center_axis',(1.22464679914735E-16,-1.,0.));
#1846=DIRECTION('ref_axis',(-1.,-1.22464679914735E-16,0.));
#1847=DIRECTION('center_axis',(0.,0.,-1.));
#1848=DIRECTION('ref_axis',(-1.,0.,0.));
#1849=DIRECTION('center_axis',(0.,0.,-1.));
#1850=DIRECTION('ref_axis',(-1.,0.,0.));
#1851=DIRECTION('center_axis',(0.,0.,1.));
#1852=DIRECTION('ref_axis',(0.653358928956991,0.757048287728183,0.));
#1853=DIRECTION('center_axis',(0.,0.,-1.));
#1854=DIRECTION('ref_axis',(-0.901632299434182,-0.432503406480261,0.));
#1855=DIRECTION('center_axis',(0.,0.,1.));
#1856=DIRECTION('ref_axis',(1.,0.,0.));
#1857=DIRECTION('',(0.880471099922175,1.07826611426144E-16,-0.474099823035018));
#1858=DIRECTION('center_axis',(0.,0.,-1.));
#1859=DIRECTION('ref_axis',(-1.,0.,0.));
#1860=DIRECTION('',(-0.880471099922175,1.07826611426144E-16,0.474099823035018));
#1861=DIRECTION('center_axis',(0.,0.,-1.));
#1862=DIRECTION('ref_axis',(-1.,0.,0.));
#1863=DIRECTION('center_axis',(0.,0.,1.));
#1864=DIRECTION('ref_axis',(1.,0.,0.));
#1865=DIRECTION('center_axis',(0.,0.,1.));
#1866=DIRECTION('ref_axis',(1.,0.,0.));
#1867=DIRECTION('center_axis',(-0.866025403784438,0.500000000000001,0.));
#1868=DIRECTION('ref_axis',(-0.500000000000001,-0.866025403784438,0.));
#1869=DIRECTION('',(0.,0.,-1.));
#1870=DIRECTION('',(0.,0.,-1.));
#1871=DIRECTION('center_axis',(-0.866025403784439,-0.499999999999999,0.));
#1872=DIRECTION('ref_axis',(0.499999999999999,-0.866025403784439,0.));
#1873=DIRECTION('',(0.,0.,-1.));
#1874=DIRECTION('center_axis',(0.,-1.,0.));
#1875=DIRECTION('ref_axis',(0.,0.,-1.));
#1876=DIRECTION('',(0.,0.,-1.));
#1877=DIRECTION('center_axis',(0.866025403784439,-0.5,0.));
#1878=DIRECTION('ref_axis',(0.5,0.866025403784439,0.));
#1879=DIRECTION('',(0.,0.,-1.));
#1880=DIRECTION('center_axis',(0.866025403784438,0.500000000000001,0.));
#1881=DIRECTION('ref_axis',(-0.500000000000001,0.866025403784438,0.));
#1882=DIRECTION('',(0.,0.,-1.));
#1883=DIRECTION('center_axis',(-1.00154306582477E-15,1.,0.));
#1884=DIRECTION('ref_axis',(-1.,-1.00154306582477E-15,0.));
#1885=DIRECTION('',(0.,0.,1.));
#1886=DIRECTION('',(1.,0.,0.));
#1887=DIRECTION('',(4.66760026650052E-14,-6.94576695567485E-14,1.));
#1888=DIRECTION('',(0.994377352516455,0.105894668432196,-3.9058363068294E-14));
#1889=DIRECTION('',(-0.105894668432205,0.994377352516455,1.96547772153004E-13));
#1890=DIRECTION('',(0.99347289286377,0.105798349409253,0.0426417683400746));
#1891=DIRECTION('',(0.226328714341839,0.0241025241588697,-0.973752731135344));
#1892=DIRECTION('',(-0.105894668432382,0.994377352516436,1.06776308541549E-13));
#1893=DIRECTION('',(0.461320952354723,0.049127656786222,0.885872142161174));
#1894=DIRECTION('',(0.105894668432382,-0.994377352516436,-1.06674624498823E-13));
#1895=DIRECTION('',(-0.105894668432184,0.994377352516457,5.32298623014658E-14));
#1896=DIRECTION('',(0.989604844221389,0.105386427589599,-0.0978567993215713));
#1897=DIRECTION('',(-0.783336483120871,-0.0834201995258221,-0.615974857054164));
#1898=DIRECTION('',(0.105894668432196,-0.994377352516456,-7.40529596891861E-14));
#1899=DIRECTION('',(-0.105894668432196,0.994377352516456,7.40117272447346E-14));
#1900=DIRECTION('',(0.993472892863762,0.105798349409249,0.04264176834028));
#1901=DIRECTION('',(-0.768139624603164,-0.0818018337315166,-0.635035414061823));
#1902=DIRECTION('',(0.105894668432196,-0.994377352516456,-7.40228494730121E-14));
#1903=DIRECTION('',(0.105894668432268,-0.994377352516448,-1.31868954441575E-13));
#1904=DIRECTION('',(0.989695401659938,0.105396071363133,0.0969261578439518));
#1905=DIRECTION('',(0.105894668432196,-0.994377352516456,-7.40101353027652E-14));
#1906=DIRECTION('',(-0.771457012031802,-0.0821551137423911,0.630955320029033));
#1907=DIRECTION('',(-0.105894668432196,0.994377352516456,7.40031184217983E-14));
#1908=DIRECTION('',(0.174958554306962,0.0186319389221334,0.984399489601056));
#1909=DIRECTION('',(-3.37175882090003E-18,-2.50033924253382E-20,1.));
#1910=DIRECTION('',(0.0451692998499449,-0.998979346308554,1.27322112582369E-19));
#1911=DIRECTION('',(0.105894668432196,-0.994377352516456,-7.40026151975994E-14));
#1912=DIRECTION('',(0.777943394083694,0.0828458709031117,-0.622848807718091));
#1913=DIRECTION('',(0.105894668432041,-0.994377352516472,-1.66959913476817E-13));
#1914=DIRECTION('',(0.98863797812138,0.105283462689014,0.107286255877818));
#1915=CARTESIAN_POINT('',(0.,0.,0.));
#1916=CARTESIAN_POINT('',(0.,0.,0.));
#1917=CARTESIAN_POINT('Origin',(-20.,-3.46944695195361E-15,0.));
#1918=CARTESIAN_POINT('',(-5.,-2.55038338414727E-16,-1.83697019872103E-15));
#1919=CARTESIAN_POINT('Origin',(0.,-4.93038065763132E-31,-2.44929359829471E-15));
#1920=CARTESIAN_POINT('Origin',(-20.,-4.08177035152729E-15,0.));
#1921=CARTESIAN_POINT('',(-25.,-4.,-22.4499443206436));
#1922=CARTESIAN_POINT('',(-25.,4.,-22.4499443206436));
#1923=CARTESIAN_POINT('Ctrl Pts',(-25.,-3.99999999999891,-22.4499443206451));
#1924=CARTESIAN_POINT('Ctrl Pts',(-25.,-3.84867032046629,-22.6566609508832));
#1925=CARTESIAN_POINT('Ctrl Pts',(-25.,-3.6835445374341,-22.848437982591));
#1926=CARTESIAN_POINT('Ctrl Pts',(-25.,-3.300301175418,-23.2366874901609));
#1927=CARTESIAN_POINT('Ctrl Pts',(-25.,-3.04126350020025,-23.4558741060066));
#1928=CARTESIAN_POINT('Ctrl Pts',(-25.,-2.48262666767397,-23.8342495941587));
#1929=CARTESIAN_POINT('Ctrl Pts',(-25.,-2.18300887639722,-23.9934109543844));
#1930=CARTESIAN_POINT('Ctrl Pts',(-25.,-1.61519723056183,-24.2312903430839));
#1931=CARTESIAN_POINT('Ctrl Pts',(-25.,-1.29504313685635,-24.3324786024398));
#1932=CARTESIAN_POINT('Ctrl Pts',(-25.,-0.640546152188757,-24.464287836246));
#1933=CARTESIAN_POINT('Ctrl Pts',(-25.,-0.306200968881558,-24.4948974278318));
#1934=CARTESIAN_POINT('Ctrl Pts',(-25.,-4.31946145518225E-15,-24.4948974278318));
#1935=CARTESIAN_POINT('Ctrl Pts',(-25.,0.30620096888155,-24.4948974278318));
#1936=CARTESIAN_POINT('Ctrl Pts',(-25.,0.64054615218875,-24.464287836246));
#1937=CARTESIAN_POINT('Ctrl Pts',(-25.,1.29504313685634,-24.3324786024398));
#1938=CARTESIAN_POINT('Ctrl Pts',(-25.,1.61519723056182,-24.2312903430839));
#1939=CARTESIAN_POINT('Ctrl Pts',(-25.,2.18300887639721,-23.9934109543844));
#1940=CARTESIAN_POINT('Ctrl Pts',(-25.,2.48262666767396,-23.8342495941587));
#1941=CARTESIAN_POINT('Ctrl Pts',(-25.,3.04126350020024,-23.4558741060066));
#1942=CARTESIAN_POINT('Ctrl Pts',(-25.,3.30030117541799,-23.2366874901609));
#1943=CARTESIAN_POINT('Ctrl Pts',(-25.,3.68354453743409,-22.848437982591));
#1944=CARTESIAN_POINT('Ctrl Pts',(-25.,3.84867032046629,-22.6566609508832));
#1945=CARTESIAN_POINT('Ctrl Pts',(-25.,3.99999999999891,-22.4499443206451));
#1946=CARTESIAN_POINT('',(-15.,-4.,-22.4499443206436));
#1947=CARTESIAN_POINT('Origin',(-20.,-4.,0.));
#1948=CARTESIAN_POINT('',(-15.,4.,-22.4499443206436));
#1949=CARTESIAN_POINT('Ctrl Pts',(-15.,-3.99999999999891,-22.4499443206451));
#1950=CARTESIAN_POINT('Ctrl Pts',(-15.,-3.84867032046629,-22.6566609508833));
#1951=CARTESIAN_POINT('Ctrl Pts',(-15.,-3.68354453743409,-22.848437982591));
#1952=CARTESIAN_POINT('Ctrl Pts',(-15.,-3.30030117541799,-23.2366874901609));
#1953=CARTESIAN_POINT('Ctrl Pts',(-15.,-3.04126350020025,-23.4558741060066));
#1954=CARTESIAN_POINT('Ctrl Pts',(-15.,-2.48262666767397,-23.8342495941587));
#1955=CARTESIAN_POINT('Ctrl Pts',(-15.,-2.18300887639722,-23.9934109543844));
#1956=CARTESIAN_POINT('Ctrl Pts',(-15.,-1.61519723056182,-24.2312903430839));
#1957=CARTESIAN_POINT('Ctrl Pts',(-15.,-1.29504313685635,-24.3324786024398));
#1958=CARTESIAN_POINT('Ctrl Pts',(-15.,-0.640546152188757,-24.464287836246));
#1959=CARTESIAN_POINT('Ctrl Pts',(-15.,-0.306200968881557,-24.4948974278318));
#1960=CARTESIAN_POINT('Ctrl Pts',(-15.,-2.60208521396521E-15,-24.4948974278318));
#1961=CARTESIAN_POINT('Ctrl Pts',(-15.,0.306200968881551,-24.4948974278318));
#1962=CARTESIAN_POINT('Ctrl Pts',(-15.,0.64054615218875,-24.464287836246));
#1963=CARTESIAN_POINT('Ctrl Pts',(-15.,1.29504313685634,-24.3324786024398));
#1964=CARTESIAN_POINT('Ctrl Pts',(-15.,1.61519723056182,-24.2312903430839));
#1965=CARTESIAN_POINT('Ctrl Pts',(-15.,2.18300887639722,-23.9934109543844));
#1966=CARTESIAN_POINT('Ctrl Pts',(-15.,2.48262666767396,-23.8342495941587));
#1967=CARTESIAN_POINT('Ctrl Pts',(-15.,3.04126350020024,-23.4558741060066));
#1968=CARTESIAN_POINT('Ctrl Pts',(-15.,3.30030117541799,-23.2366874901609));
#1969=CARTESIAN_POINT('Ctrl Pts',(-15.,3.68354453743409,-22.848437982591));
#1970=CARTESIAN_POINT('Ctrl Pts',(-15.,3.84867032046629,-22.6566609508832));
#1971=CARTESIAN_POINT('Ctrl Pts',(-15.,3.99999999999891,-22.4499443206451));
#1972=CARTESIAN_POINT('Origin',(-20.,4.,0.));
#1973=CARTESIAN_POINT('Origin',(-20.,0.,-51.));
#1974=CARTESIAN_POINT('',(-20.,4.,-28.));
#1975=CARTESIAN_POINT('',(-20.,-4.,-28.));
#1976=CARTESIAN_POINT('Origin',(-20.,0.,-28.));
#1977=CARTESIAN_POINT('',(-24.,-4.89858719658941E-16,-28.));
#1978=CARTESIAN_POINT('Origin',(-20.,0.,-28.));
#1979=CARTESIAN_POINT('',(-24.,-4.89858719658941E-16,-51.));
#1980=CARTESIAN_POINT('',(-24.,-4.89858719658941E-16,-51.));
#1981=CARTESIAN_POINT('Origin',(-20.,0.,-51.));
#1982=CARTESIAN_POINT('Origin',(-20.,0.,-28.));
#1983=CARTESIAN_POINT('Origin',(0.,0.,-28.));
#1984=CARTESIAN_POINT('',(-15.,4.,-28.));
#1985=CARTESIAN_POINT('',(-15.,4.,-28.));
#1986=CARTESIAN_POINT('',(-15.,-4.,-28.));
#1987=CARTESIAN_POINT('',(-15.,0.,-28.));
#1988=CARTESIAN_POINT('',(-25.,-4.,-28.));
#1989=CARTESIAN_POINT('Origin',(0.,0.,-28.));
#1990=CARTESIAN_POINT('',(-25.,-4.,-28.));
#1991=CARTESIAN_POINT('',(-25.,-4.,-28.));
#1992=CARTESIAN_POINT('',(-25.,4.,-28.));
#1993=CARTESIAN_POINT('',(-25.,4.,-28.));
#1994=CARTESIAN_POINT('',(-15.,4.,-28.));
#1995=CARTESIAN_POINT('Origin',(-15.,0.,-18.));
#1996=CARTESIAN_POINT('',(-15.,4.,-18.));
#1997=CARTESIAN_POINT('',(-15.,-4.,-18.));
#1998=CARTESIAN_POINT('Origin',(-15.,4.,-18.));
#1999=CARTESIAN_POINT('',(-25.,4.,-18.));
#2000=CARTESIAN_POINT('Origin',(-25.,4.,-18.));
#2001=CARTESIAN_POINT('',(-25.,-4.,-18.));
#2002=CARTESIAN_POINT('Origin',(-25.,-4.,-18.));
#2003=CARTESIAN_POINT('Origin',(-20.,0.,-51.));
#2004=CARTESIAN_POINT('',(0.,0.,0.));
#2005=CARTESIAN_POINT('Origin',(-3.17155304177845E-15,-9.50000000000001,
7.));
#2006=CARTESIAN_POINT('',(4.5,-9.00000000000001,7.));
#2007=CARTESIAN_POINT('Origin',(-3.00462919747432E-15,-9.00000000000001,
7.));
#2008=CARTESIAN_POINT('',(4.,-9.50000000000001,7.));
#2009=CARTESIAN_POINT('Origin',(4.5,-9.50000000000001,7.));
#2010=CARTESIAN_POINT('Origin',(-3.17155304177845E-15,-9.50000000000001,
7.));
#2011=CARTESIAN_POINT('Origin',(-7.28523761486083E-16,9.50000000000003,
7.));
#2012=CARTESIAN_POINT('',(-4.5,9.00000000000002,7.));
#2013=CARTESIAN_POINT('Origin',(-6.45061839334019E-16,9.00000000000002,
7.));
#2014=CARTESIAN_POINT('',(-4.,9.50000000000002,7.));
#2015=CARTESIAN_POINT('Origin',(-4.5,9.50000000000003,7.));
#2016=CARTESIAN_POINT('Origin',(-7.28523761486083E-16,9.50000000000003,
7.));
#2017=CARTESIAN_POINT('Origin',(-6.51002992786103E-15,-19.5,7.));
#2018=CARTESIAN_POINT('',(3.99999999999999,-19.5,7.));
#2019=CARTESIAN_POINT('',(3.99999999999999,-19.5,7.));
#2020=CARTESIAN_POINT('Origin',(-6.51002992786103E-15,-19.5,7.));
#2021=CARTESIAN_POINT('Origin',(-2.39776220452737E-15,19.5,7.));
#2022=CARTESIAN_POINT('',(-4.,19.5,7.));
#2023=CARTESIAN_POINT('',(-4.,19.5,7.));
#2024=CARTESIAN_POINT('Origin',(-2.39776220452737E-15,19.5,7.));
#2025=CARTESIAN_POINT('Origin',(0.,0.,14.));
#2026=CARTESIAN_POINT('',(4.5,-5.51091059616309E-16,14.));
#2027=CARTESIAN_POINT('Origin',(0.,0.,14.));
#2028=CARTESIAN_POINT('',(4.5,-5.51091059616309E-16,0.));
#2029=CARTESIAN_POINT('',(4.5,-5.51091059616309E-16,14.));
#2030=CARTESIAN_POINT('Origin',(0.,0.,0.));
#2031=CARTESIAN_POINT('Origin',(-5.19615242270664,-9.00000000000001,14.));
#2032=CARTESIAN_POINT('',(-5.19615242270664,-9.00000000000001,0.));
#2033=CARTESIAN_POINT('',(5.19615242270663,-9.00000000000001,0.));
#2034=CARTESIAN_POINT('',(-5.19615242270664,-9.00000000000001,0.));
#2035=CARTESIAN_POINT('',(5.19615242270663,-9.00000000000001,14.));
#2036=CARTESIAN_POINT('',(5.19615242270663,-9.00000000000001,14.));
#2037=CARTESIAN_POINT('',(-5.19615242270664,-9.00000000000001,14.));
#2038=CARTESIAN_POINT('',(-5.19615242270664,-9.00000000000001,14.));
#2039=CARTESIAN_POINT('',(-5.19615242270664,-9.00000000000001,14.));
#2040=CARTESIAN_POINT('Origin',(5.19615242270661,9.00000000000002,14.));
#2041=CARTESIAN_POINT('',(5.19615242270661,9.00000000000002,0.));
#2042=CARTESIAN_POINT('',(-5.19615242270664,9.00000000000002,0.));
#2043=CARTESIAN_POINT('',(5.19615242270661,9.00000000000002,0.));
#2044=CARTESIAN_POINT('',(-5.19615242270664,9.00000000000002,14.));
#2045=CARTESIAN_POINT('',(-5.19615242270664,9.00000000000002,14.));
#2046=CARTESIAN_POINT('',(5.19615242270661,9.00000000000002,14.));
#2047=CARTESIAN_POINT('',(5.19615242270661,9.00000000000002,14.));
#2048=CARTESIAN_POINT('',(5.19615242270661,9.00000000000002,14.));
#2049=CARTESIAN_POINT('Origin',(0.,0.,14.));
#2050=CARTESIAN_POINT('',(10.3923048454133,7.03904010014224E-16,14.));
#2051=CARTESIAN_POINT('',(5.19615242270663,-9.00000000000001,14.));
#2052=CARTESIAN_POINT('',(10.3923048454133,7.03904010014224E-16,14.));
#2053=CARTESIAN_POINT('',(-10.3923048454133,-8.2724230250131E-16,14.));
#2054=CARTESIAN_POINT('',(-5.19615242270664,9.00000000000002,14.));
#2055=CARTESIAN_POINT('',(-10.3923048454133,-8.2724230250131E-16,14.));
#2056=CARTESIAN_POINT('Origin',(0.,0.,0.));
#2057=CARTESIAN_POINT('',(10.3923048454133,7.03904010014224E-16,0.));
#2058=CARTESIAN_POINT('',(5.19615242270663,-9.00000000000001,0.));
#2059=CARTESIAN_POINT('',(-10.3923048454133,-8.2724230250131E-16,0.));
#2060=CARTESIAN_POINT('',(-10.3923048454133,-8.2724230250131E-16,0.));
#2061=CARTESIAN_POINT('',(-5.19615242270664,9.00000000000002,0.));
#2062=CARTESIAN_POINT('',(10.3923048454133,7.03904010014224E-16,0.));
#2063=CARTESIAN_POINT('Origin',(5.19615242270663,-9.00000000000001,14.));
#2064=CARTESIAN_POINT('',(10.3923048454133,7.03904010014224E-16,14.));
#2065=CARTESIAN_POINT('Origin',(10.3923048454133,7.03904010014224E-16,14.));
#2066=CARTESIAN_POINT('Origin',(-5.19615242270664,9.00000000000002,14.));
#2067=CARTESIAN_POINT('',(-10.3923048454133,-8.2724230250131E-16,14.));
#2068=CARTESIAN_POINT('Origin',(-10.3923048454133,-8.2724230250131E-16,
14.));
#2069=CARTESIAN_POINT('Origin',(-2.39776220452737E-15,19.5,7.));
#2070=CARTESIAN_POINT('Origin',(-6.51002992786103E-15,-19.5,7.));
#2071=CARTESIAN_POINT('',(0.,0.,0.));
#2072=CARTESIAN_POINT('Origin',(9.5,0.,0.));
#2073=CARTESIAN_POINT('',(9.,-5.51091059616309E-16,-4.5));
#2074=CARTESIAN_POINT('Origin',(9.,0.,0.));
#2075=CARTESIAN_POINT('',(9.5,-4.89858719658941E-16,-4.));
#2076=CARTESIAN_POINT('Origin',(9.5,-5.51091059616309E-16,-4.5));
#2077=CARTESIAN_POINT('Origin',(9.5,0.,0.));
#2078=CARTESIAN_POINT('Origin',(-9.5,0.,0.));
#2079=CARTESIAN_POINT('',(-9.,5.51091059616309E-16,-4.5));
#2080=CARTESIAN_POINT('',(-9.,-5.51091059616309E-16,4.5));
#2081=CARTESIAN_POINT('Origin',(-9.,0.,0.));
#2082=CARTESIAN_POINT('',(-9.5,-4.89858719658941E-16,4.));
#2083=CARTESIAN_POINT('Origin',(-9.5,-5.51091059616309E-16,4.5));
#2084=CARTESIAN_POINT('',(-9.5,4.89858719658941E-16,-4.));
#2085=CARTESIAN_POINT('Origin',(-9.5,0.,0.));
#2086=CARTESIAN_POINT('Origin',(-9.5,0.,0.));
#2087=CARTESIAN_POINT('Origin',(-9.,0.,0.));
#2088=CARTESIAN_POINT('Origin',(-25.,0.,0.));
#2089=CARTESIAN_POINT('',(-25.,-4.89858719658941E-16,-4.));
#2090=CARTESIAN_POINT('Origin',(-25.,0.,0.));
#2091=CARTESIAN_POINT('',(-25.,-4.89858719658941E-16,-4.));
#2092=CARTESIAN_POINT('Origin',(-25.,0.,0.));
#2093=CARTESIAN_POINT('',(-25.,-5.51091059616309E-16,-4.5));
#2094=CARTESIAN_POINT('Origin',(-25.,0.,0.));
#2095=CARTESIAN_POINT('',(25.,-4.89858719658941E-16,-4.));
#2096=CARTESIAN_POINT('',(-25.,-4.89858719658941E-16,-4.));
#2097=CARTESIAN_POINT('Origin',(25.,0.,0.));
#2098=CARTESIAN_POINT('Origin',(25.,0.,0.));
#2099=CARTESIAN_POINT('Origin',(-25.,0.,0.));
#2100=CARTESIAN_POINT('',(0.,0.,0.));
#2101=CARTESIAN_POINT('Origin',(0.,0.,5.));
#2102=CARTESIAN_POINT('',(4.,-4.89858719658941E-16,5.));
#2103=CARTESIAN_POINT('Origin',(0.,0.,5.));
#2104=CARTESIAN_POINT('',(4.,-4.89858719658941E-16,0.));
#2105=CARTESIAN_POINT('',(4.,-4.89858719658941E-16,5.));
#2106=CARTESIAN_POINT('Origin',(0.,0.,0.));
#2107=CARTESIAN_POINT('Origin',(24.,44.00000032792,5.));
#2108=CARTESIAN_POINT('',(28.,44.00000032792,5.));
#2109=CARTESIAN_POINT('Origin',(24.,44.00000032792,5.));
#2110=CARTESIAN_POINT('',(28.,44.00000032792,0.));
#2111=CARTESIAN_POINT('',(28.,44.00000032792,5.));
#2112=CARTESIAN_POINT('Origin',(24.,44.00000032792,0.));
#2113=CARTESIAN_POINT('Origin',(-24.,44.00000032792,5.));
#2114=CARTESIAN_POINT('',(-20.,44.00000032792,5.));
#2115=CARTESIAN_POINT('Origin',(-24.,44.00000032792,5.));
#2116=CARTESIAN_POINT('',(-20.,44.00000032792,0.));
#2117=CARTESIAN_POINT('',(-20.,44.00000032792,5.));
#2118=CARTESIAN_POINT('Origin',(-24.,44.00000032792,0.));
#2119=CARTESIAN_POINT('Origin',(-24.,44.00000032792,5.));
#2120=CARTESIAN_POINT('',(-24.,54.00000032792,5.));
#2121=CARTESIAN_POINT('',(-32.7789556978139,39.2114789636761,5.));
#2122=CARTESIAN_POINT('Origin',(-24.,44.00000032792,5.));
#2123=CARTESIAN_POINT('',(-24.,54.00000032792,0.));
#2124=CARTESIAN_POINT('',(-24.,54.00000032792,5.));
#2125=CARTESIAN_POINT('',(-32.7789556978139,39.2114789636761,0.));
#2126=CARTESIAN_POINT('Origin',(-24.,44.00000032792,0.));
#2127=CARTESIAN_POINT('',(-32.7789556978139,39.2114789636761,5.));
#2128=CARTESIAN_POINT('Origin',(-24.,44.00000032792,5.));
#2129=CARTESIAN_POINT('',(-8.77895527208265,-4.7885211320269,5.));
#2130=CARTESIAN_POINT('',(-32.7789556978139,39.2114789636761,5.));
#2131=CARTESIAN_POINT('',(8.77895544126431,-4.78852082186052,5.));
#2132=CARTESIAN_POINT('Origin',(0.,0.,5.));
#2133=CARTESIAN_POINT('',(32.7789556978139,39.2114789636761,5.));
#2134=CARTESIAN_POINT('',(8.77895544126431,-4.78852082186051,5.));
#2135=CARTESIAN_POINT('',(24.,54.00000032792,5.));
#2136=CARTESIAN_POINT('Origin',(24.,44.00000032792,5.));
#2137=CARTESIAN_POINT('',(24.,54.00000032792,5.));
#2138=CARTESIAN_POINT('Origin',(-24.,44.00000032792,0.));
#2139=CARTESIAN_POINT('',(24.,54.00000032792,0.));
#2140=CARTESIAN_POINT('',(24.,54.00000032792,0.));
#2141=CARTESIAN_POINT('',(32.7789556978139,39.2114789636761,0.));
#2142=CARTESIAN_POINT('Origin',(24.,44.00000032792,0.));
#2143=CARTESIAN_POINT('',(8.77895544126431,-4.78852082186052,0.));
#2144=CARTESIAN_POINT('',(8.77895544126431,-4.78852082186051,0.));
#2145=CARTESIAN_POINT('',(-8.77895527208265,-4.7885211320269,0.));
#2146=CARTESIAN_POINT('Origin',(0.,0.,0.));
#2147=CARTESIAN_POINT('',(-32.7789556978139,39.2114789636761,0.));
#2148=CARTESIAN_POINT('Origin',(-32.7789556978139,39.2114789636761,5.));
#2149=CARTESIAN_POINT('',(-8.77895527208265,-4.7885211320269,5.));
#2150=CARTESIAN_POINT('Origin',(0.,0.,5.));
#2151=CARTESIAN_POINT('',(8.77895544126431,-4.78852082186052,5.));
#2152=CARTESIAN_POINT('Origin',(8.77895544126431,-4.78852082186051,5.));
#2153=CARTESIAN_POINT('',(32.7789556978139,39.2114789636761,5.));
#2154=CARTESIAN_POINT('Origin',(24.,44.00000032792,5.));
#2155=CARTESIAN_POINT('',(24.,54.00000032792,5.));
#2156=CARTESIAN_POINT('Origin',(24.,54.00000032792,5.));
#2157=CARTESIAN_POINT('',(0.,0.,0.));
#2158=CARTESIAN_POINT('Origin',(-8.50000000000001,0.,0.));
#2159=CARTESIAN_POINT('',(-6.50000000000001,-9.79717439317883E-16,8.));
#2160=CARTESIAN_POINT('Origin',(-6.50000000000001,0.,0.));
#2161=CARTESIAN_POINT('',(-8.50000000000001,-9.79717439317883E-16,8.));
#2162=CARTESIAN_POINT('',(-8.50000000000001,-9.79717439317883E-16,8.));
#2163=CARTESIAN_POINT('Origin',(-8.50000000000001,0.,0.));
#2164=CARTESIAN_POINT('Origin',(-8.50000000000001,0.,0.));
#2165=CARTESIAN_POINT('',(-4.50000000000001,-2.44929359829471E-15,20.));
#2166=CARTESIAN_POINT('Origin',(-4.50000000000001,0.,0.));
#2167=CARTESIAN_POINT('',(-6.50000000000001,-2.44929359829471E-15,20.));
#2168=CARTESIAN_POINT('',(-8.50000000000001,-2.44929359829471E-15,20.));
#2169=CARTESIAN_POINT('Origin',(-6.50000000000001,0.,0.));
#2170=CARTESIAN_POINT('Origin',(-8.50000000000001,0.,0.));
#2171=CARTESIAN_POINT('',(4.50000000000001,-2.0818995585505E-15,17.));
#2172=CARTESIAN_POINT('Origin',(4.50000000000001,0.,0.));
#2173=CARTESIAN_POINT('',(-4.50000000000001,-2.0818995585505E-15,17.));
#2174=CARTESIAN_POINT('',(-8.50000000000001,-2.0818995585505E-15,17.));
#2175=CARTESIAN_POINT('Origin',(-4.50000000000001,0.,0.));
#2176=CARTESIAN_POINT('Origin',(-8.50000000000001,0.,0.));
#2177=CARTESIAN_POINT('',(6.50000000000001,-2.44929359829471E-15,20.));
#2178=CARTESIAN_POINT('Origin',(6.50000000000001,0.,0.));
#2179=CARTESIAN_POINT('',(4.50000000000001,-2.44929359829471E-15,20.));
#2180=CARTESIAN_POINT('',(-8.50000000000001,-2.44929359829471E-15,20.));
#2181=CARTESIAN_POINT('Origin',(4.50000000000001,0.,0.));
#2182=CARTESIAN_POINT('Origin',(-8.50000000000001,0.,0.));
#2183=CARTESIAN_POINT('',(8.50000000000001,-9.79717439317883E-16,8.));
#2184=CARTESIAN_POINT('Origin',(8.50000000000001,0.,0.));
#2185=CARTESIAN_POINT('',(6.50000000000001,-9.79717439317883E-16,8.));
#2186=CARTESIAN_POINT('',(-8.50000000000001,-9.79717439317883E-16,8.));
#2187=CARTESIAN_POINT('Origin',(6.50000000000001,0.,0.));
#2188=CARTESIAN_POINT('Origin',(-8.50000000000001,0.,0.));
#2189=CARTESIAN_POINT('',(-8.50000000000001,-5.51091059616309E-16,4.5));
#2190=CARTESIAN_POINT('Origin',(-8.50000000000001,0.,0.));
#2191=CARTESIAN_POINT('',(8.50000000000001,-5.51091059616309E-16,4.5));
#2192=CARTESIAN_POINT('',(-8.50000000000001,-5.51091059616309E-16,4.5));
#2193=CARTESIAN_POINT('Origin',(8.50000000000001,0.,0.));
#2194=CARTESIAN_POINT('Origin',(8.50000000000001,0.,0.));
#2195=CARTESIAN_POINT('Origin',(6.50000000000001,0.,0.));
#2196=CARTESIAN_POINT('Origin',(4.50000000000001,0.,0.));
#2197=CARTESIAN_POINT('Origin',(-4.50000000000001,0.,0.));
#2198=CARTESIAN_POINT('Origin',(-6.50000000000001,0.,0.));
#2199=CARTESIAN_POINT('Origin',(-8.50000000000001,0.,0.));
#2200=CARTESIAN_POINT('',(0.,0.,0.));
#2201=CARTESIAN_POINT('Origin',(0.,0.,6.));
#2202=CARTESIAN_POINT('',(3.4,1.886685021085E-13,1.93750000000002));
#2203=CARTESIAN_POINT('',(3.4,-1.7333563370988E-13,1.92749999999998));
#2204=CARTESIAN_POINT('',(3.4,-4.163799117101E-16,6.));
#2205=CARTESIAN_POINT('',(3.37685862035149,0.396012446973337,0.700000000000002));
#2206=CARTESIAN_POINT('Ctrl Pts',(3.4,-3.4625488750805E-13,1.92749999999998));
#2207=CARTESIAN_POINT('Ctrl Pts',(3.39999999999999,-0.0751214124647497,
1.92333274051478));
#2208=CARTESIAN_POINT('Ctrl Pts',(3.39751039970816,-0.150316128865589,1.91910420870307));
#2209=CARTESIAN_POINT('Ctrl Pts',(3.36253534799724,-0.676583934114712,1.88910655418598));
#2210=CARTESIAN_POINT('Ctrl Pts',(3.24287468221216,-1.11718618023821,1.86191518047301));
#2211=CARTESIAN_POINT('Ctrl Pts',(2.84552536189263,-1.91128615387662,1.80873328142527));
#2212=CARTESIAN_POINT('Ctrl Pts',(2.57731571088716,-2.25995921897011,1.78416891830816));
#2213=CARTESIAN_POINT('Ctrl Pts',(1.91158513943287,-2.84788181098038,1.73372915804847));
#2214=CARTESIAN_POINT('Ctrl Pts',(1.51622136776119,-3.07661995617186,1.70654095205508));
#2215=CARTESIAN_POINT('Ctrl Pts',(0.674677953708942,-3.36078822430551,1.65332785941573));
#2216=CARTESIAN_POINT('Ctrl Pts',(0.238650846294366,-3.41951310237242,1.62868720616195));
#2217=CARTESIAN_POINT('Ctrl Pts',(-0.648283414878094,-3.36815779516296,
1.5783056797496));
#2218=CARTESIAN_POINT('Ctrl Pts',(-1.09025108249999,-3.25208205777719,1.55112093538634));
#2219=CARTESIAN_POINT('Ctrl Pts',(-1.88804380928579,-2.86102085156782,1.49787867373243));
#2220=CARTESIAN_POINT('Ctrl Pts',(-2.23899450631159,-2.59556991721883,1.47316327182734));
#2221=CARTESIAN_POINT('Ctrl Pts',(-2.8325994386573,-1.93424395427837,1.42283728282858));
#2222=CARTESIAN_POINT('Ctrl Pts',(-3.06464870302035,-1.54038056751001,1.39565622597147));
#2223=CARTESIAN_POINT('Ctrl Pts',(-3.35550133962885,-0.700588956999663,
1.34238671925571));
#2224=CARTESIAN_POINT('Ctrl Pts',(-3.41759775458745,-0.264883297406569,
1.31759840541435));
#2225=CARTESIAN_POINT('Ctrl Pts',(-3.37299216600685,0.622892781759607,1.26732527491678));
#2226=CARTESIAN_POINT('Ctrl Pts',(-3.26013973203468,1.06605967034742,1.24014807025696));
#2227=CARTESIAN_POINT('Ctrl Pts',(-2.87472803373432,1.86714190123431,1.18685314184052));
#2228=CARTESIAN_POINT('Ctrl Pts',(-2.61174512528069,2.2201316660374,1.16199399900912));
#2229=CARTESIAN_POINT('Ctrl Pts',(-1.95437463831632,2.81880032541014,1.11177108070705));
#2230=CARTESIAN_POINT('Ctrl Pts',(-1.56187370908267,3.05379875999433,1.08459783849235));
#2231=CARTESIAN_POINT('Ctrl Pts',(-0.723668687168632,3.35061944763769,1.03127921212292));
#2232=CARTESIAN_POINT('Ctrl Pts',(-0.288248857360501,3.415723993581,1.00635152330788));
#2233=CARTESIAN_POINT('Ctrl Pts',(0.600256135722737,3.37713545522293,0.956176216715607));
#2234=CARTESIAN_POINT('Ctrl Pts',(1.04447166788701,3.26716227445194,0.929006999272162));
#2235=CARTESIAN_POINT('Ctrl Pts',(1.84846805982719,2.88679407269544,0.875666300851262));
#2236=CARTESIAN_POINT('Ctrl Pts',(2.20327250640915,2.62600628040714,0.850672506218438));
#2237=CARTESIAN_POINT('Ctrl Pts',(2.74028398997315,2.04386855383655,0.806039779237286));
#2238=CARTESIAN_POINT('Ctrl Pts',(2.93894310375689,1.74617193811401,0.784960681789362));
#2239=CARTESIAN_POINT('Ctrl Pts',(3.23761590955786,1.0981423198909,0.742149222714576));
#2240=CARTESIAN_POINT('Ctrl Pts',(3.33517029647866,0.751495151908227,0.720677837576191));
#2241=CARTESIAN_POINT('Ctrl Pts',(3.37685862035149,0.396012446973369,0.700000000000005));
#2242=CARTESIAN_POINT('',(3.39272377138046,0.222318265353878,0.700000000000003));
#2243=CARTESIAN_POINT('Origin',(0.,0.,0.700000000000003));
#2244=CARTESIAN_POINT('Ctrl Pts',(3.39272377138046,0.222318265353877,0.700000000000002));
#2245=CARTESIAN_POINT('Ctrl Pts',(3.37412547491926,0.506140570330221,0.716172011820753));
#2246=CARTESIAN_POINT('Ctrl Pts',(3.31998703241798,0.786485391117649,0.732967754260724));
#2247=CARTESIAN_POINT('Ctrl Pts',(3.14234381547146,1.32971112277357,0.767184347683065));
#2248=CARTESIAN_POINT('Ctrl Pts',(3.01887224077644,1.59024336880604,0.784474146775485));
#2249=CARTESIAN_POINT('Ctrl Pts',(2.62760958855879,2.20188958075105,0.827394809286271));
#2250=CARTESIAN_POINT('Ctrl Pts',(2.32175071403847,2.5223253300443,0.851036839792356));
#2251=CARTESIAN_POINT('Ctrl Pts',(1.5999770548258,3.03286055950024,0.902807312827531));
#2252=CARTESIAN_POINT('Ctrl Pts',(1.18957513867269,3.21606383785568,0.929783442201523));
#2253=CARTESIAN_POINT('Ctrl Pts',(0.327205679871517,3.41261700251858,0.982138617014873));
#2254=CARTESIAN_POINT('Ctrl Pts',(-0.115991804276865,3.42630500609258,1.00583005470857));
#2255=CARTESIAN_POINT('Ctrl Pts',(-0.988539108930611,3.28339257492864,1.05751727823502));
#2256=CARTESIAN_POINT('Ctrl Pts',(-1.4091646726289,3.12603795168328,1.0844666018519));
#2257=CARTESIAN_POINT('Ctrl Pts',(-2.16163383983647,2.6609667424342,1.13689519739393));
#2258=CARTESIAN_POINT('Ctrl Pts',(-2.48730708019587,2.35938761807513,1.16064433579374));
#2259=CARTESIAN_POINT('Ctrl Pts',(-3.00855100939004,1.64505569074969,1.21224805261772));
#2260=CARTESIAN_POINT('Ctrl Pts',(-3.19761651264121,1.23806873692515,1.23916944340088));
#2261=CARTESIAN_POINT('Ctrl Pts',(-3.4074155924874,0.378584884973299,1.2916689069089));
#2262=CARTESIAN_POINT('Ctrl Pts',(-3.42776120331645,-0.0652819333619287,
1.31548353229742));
#2263=CARTESIAN_POINT('Ctrl Pts',(-3.29751165500039,-0.94006407528417,1.36700376344325));
#2264=CARTESIAN_POINT('Ctrl Pts',(-3.14663149078755,-1.36234659974212,1.39389623499455));
#2265=CARTESIAN_POINT('Ctrl Pts',(-2.69283660283573,-2.12199326490917,1.44646388595065));
#2266=CARTESIAN_POINT('Ctrl Pts',(-2.3954353691001,-2.45277677318083,1.4703511998463));
#2267=CARTESIAN_POINT('Ctrl Pts',(-1.68838832626413,-2.98435427657513,1.52178824174531));
#2268=CARTESIAN_POINT('Ctrl Pts',(-1.28478836071299,-3.17904312972706,1.54865095690521));
#2269=CARTESIAN_POINT('Ctrl Pts',(-0.428205698086118,-3.40166035571351,
1.60128401543907));
#2270=CARTESIAN_POINT('Ctrl Pts',(0.0163083473326349,-3.42846701123013,
1.6252505703603));
#2271=CARTESIAN_POINT('Ctrl Pts',(0.893164120516335,-3.31043983444755,1.6766049884818));
#2272=CARTESIAN_POINT('Ctrl Pts',(1.31695104779562,-3.16581130059277,1.70343726516491));
#2273=CARTESIAN_POINT('Ctrl Pts',(2.08342989700817,-2.72294177772439,1.75613287996062));
#2274=CARTESIAN_POINT('Ctrl Pts',(2.41914338179383,-2.42957489515017,1.78018452939157));
#2275=CARTESIAN_POINT('Ctrl Pts',(2.96058323228635,-1.72957694899934,1.83145714854881));
#2276=CARTESIAN_POINT('Ctrl Pts',(3.16060634091826,-1.32929335181225,1.85825846283549));
#2277=CARTESIAN_POINT('Ctrl Pts',(3.35919394319754,-0.607510420852717,1.90286153598097));
#2278=CARTESIAN_POINT('Ctrl Pts',(3.4,-0.304158067979466,1.92062723959507));
#2279=CARTESIAN_POINT('Ctrl Pts',(3.4,3.75914577244174E-13,1.93750000000002));
#2280=CARTESIAN_POINT('Origin',(0.,0.,6.));
#2281=CARTESIAN_POINT('',(3.4,2.00975518948028E-13,3.18750000000002));
#2282=CARTESIAN_POINT('',(3.4,-2.31845815703038E-13,3.17749999999997));
#2283=CARTESIAN_POINT('',(3.4,-4.163799117101E-16,6.));
#2284=CARTESIAN_POINT('Ctrl Pts',(3.4,-4.60083360298569E-13,3.17749999999997));
#2285=CARTESIAN_POINT('Ctrl Pts',(3.39999999999998,-0.124055612801236,3.17061818145879));
#2286=CARTESIAN_POINT('Ctrl Pts',(3.39321082219142,-0.248246409564226,3.16357286244051));
#2287=CARTESIAN_POINT('Ctrl Pts',(3.33116756101355,-0.811870855624036,3.13088092671118));
#2288=CARTESIAN_POINT('Ctrl Pts',(3.19734659839163,-1.23803930410971,3.10416487407304));
#2289=CARTESIAN_POINT('Ctrl Pts',(2.77346040786446,-2.01610650879456,3.05126260871194));
#2290=CARTESIAN_POINT('Ctrl Pts',(2.48707839500391,-2.36033777798621,3.02685663175361));
#2291=CARTESIAN_POINT('Ctrl Pts',(1.7929353991586,-2.92374484925883,2.97540404659579));
#2292=CARTESIAN_POINT('Ctrl Pts',(1.39026664782006,-3.1352848688268,2.94820578418326));
#2293=CARTESIAN_POINT('Ctrl Pts',(0.54010689947229,-3.3849815708294,2.8953067975875));
#2294=CARTESIAN_POINT('Ctrl Pts',(0.102397368140257,-3.42626792230477,2.87128393927437));
#2295=CARTESIAN_POINT('Ctrl Pts',(-0.779759552893679,-3.3399279964116,2.82036355488111));
#2296=CARTESIAN_POINT('Ctrl Pts',(-1.21512493198708,-3.20726728549062,2.79316397506227));
#2297=CARTESIAN_POINT('Ctrl Pts',(-1.99552112635261,-2.7870613886808,2.74021707769849));
#2298=CARTESIAN_POINT('Ctrl Pts',(-2.33583968220507,-2.50871391944311,2.71611974922401));
#2299=CARTESIAN_POINT('Ctrl Pts',(-2.90268788574612,-1.82695946513531,2.66527533163809));
#2300=CARTESIAN_POINT('Ctrl Pts',(-3.11913619711619,-1.4262931678841,2.6380753702369));
#2301=CARTESIAN_POINT('Ctrl Pts',(-3.3786317075168,-0.578512038455339,2.58508317788875));
#2302=CARTESIAN_POINT('Ctrl Pts',(-3.42488520840102,-0.141285215142229,
2.56090941845037));
#2303=CARTESIAN_POINT('Ctrl Pts',(-3.34851993642526,0.74230513788558,2.51013871335301));
#2304=CARTESIAN_POINT('Ctrl Pts',(-3.22056580886756,1.17961881649017,2.48293920183057));
#2305=CARTESIAN_POINT('Ctrl Pts',(-2.80864605558055,1.96503421009277,2.42990426964723));
#2306=CARTESIAN_POINT('Ctrl Pts',(-2.53399448601039,2.30839566056453,2.40565276182308));
#2307=CARTESIAN_POINT('Ctrl Pts',(-1.8580511213592,2.8829610420091,2.35495338177295));
#2308=CARTESIAN_POINT('Ctrl Pts',(-1.45927879698983,3.10391090200561,2.32775504965466));
#2309=CARTESIAN_POINT('Ctrl Pts',(-0.613734967667859,3.37241972842292,2.2746798610805));
#2310=CARTESIAN_POINT('Ctrl Pts',(-0.176948946422862,3.42323463003873,2.25034988916224));
#2311=CARTESIAN_POINT('Ctrl Pts',(0.707906623729064,3.35602338427,2.19971933851952));
#2312=CARTESIAN_POINT('Ctrl Pts',(1.14696212981517,3.23240453137218,2.17252281714256));
#2313=CARTESIAN_POINT('Ctrl Pts',(1.93694225593166,2.82810566485756,2.11940977484039));
#2314=CARTESIAN_POINT('Ctrl Pts',(2.28308793287607,2.55683229388904,2.09500117802721));
#2315=CARTESIAN_POINT('Ctrl Pts',(2.86467311712893,1.88623164311572,2.04443687723939));
#2316=CARTESIAN_POINT('Ctrl Pts',(3.08971677030665,1.48923000405015,2.01724270457179));
#2317=CARTESIAN_POINT('Ctrl Pts',(3.34296531938119,0.717336589060177,1.96860382359178));
#2318=CARTESIAN_POINT('Ctrl Pts',(3.40000000000004,0.359580275069644,1.9474472329236));
#2319=CARTESIAN_POINT('Ctrl Pts',(3.4,-3.45973250048814E-13,1.92749999999998));
#2320=CARTESIAN_POINT('Ctrl Pts',(3.4,3.74526798463393E-13,1.93750000000002));
#2321=CARTESIAN_POINT('Ctrl Pts',(3.4,0.136279469776807,1.94505992059303));
#2322=CARTESIAN_POINT('Ctrl Pts',(3.39180705844705,0.272699724057435,1.95281590794641));
#2323=CARTESIAN_POINT('Ctrl Pts',(3.3221402026329,0.84830236752116,1.98634749260179));
#2324=CARTESIAN_POINT('Ctrl Pts',(3.18348028608021,1.2734386993689,2.01311747915411));
#2325=CARTESIAN_POINT('Ctrl Pts',(2.75107870203134,2.04635190683021,2.06592949965133));
#2326=CARTESIAN_POINT('Ctrl Pts',(2.46156686998329,2.38676981770287,2.09016593969441));
#2327=CARTESIAN_POINT('Ctrl Pts',(1.7683141254283,2.93752419790701,2.14127840656622));
#2328=CARTESIAN_POINT('Ctrl Pts',(1.37123772364491,3.14255430517566,2.16801685651457));
#2329=CARTESIAN_POINT('Ctrl Pts',(0.520350566691976,3.3890530057568,2.22088271163742));
#2330=CARTESIAN_POINT('Ctrl Pts',(0.074636608528427,3.42795309007607,2.24521732990269));
#2331=CARTESIAN_POINT('Ctrl Pts',(-0.80585263247956,3.33261816792688,2.29625188848068));
#2332=CARTESIAN_POINT('Ctrl Pts',(-1.23218612599118,3.19959587461778,2.32295874499352));
#2333=CARTESIAN_POINT('Ctrl Pts',(-2.01109866267633,2.77711773964354,2.37587554979457));
#2334=CARTESIAN_POINT('Ctrl Pts',(-2.35595932548207,2.49125279947127,2.40031119093976));
#2335=CARTESIAN_POINT('Ctrl Pts',(-2.91542455075476,1.80438620286028,2.45126955211513));
#2336=CARTESIAN_POINT('Ctrl Pts',(-3.12510855551194,1.41037495197566,2.47794490391592));
#2337=CARTESIAN_POINT('Ctrl Pts',(-3.38249509927501,0.562211989160962,2.5309098182471));
#2338=CARTESIAN_POINT('Ctrl Pts',(-3.42693586011265,0.115955599795384,2.55544858819458));
#2339=CARTESIAN_POINT('Ctrl Pts',(-3.34191394517752,-0.766092246809965,
2.60633263665211));
#2340=CARTESIAN_POINT('Ctrl Pts',(-3.21416329916218,-1.19347755885311,2.63297670978421));
#2341=CARTESIAN_POINT('Ctrl Pts',(-2.80099829533727,-1.9779321294727,2.68598695489635));
#2342=CARTESIAN_POINT('Ctrl Pts',(-2.51855061492812,-2.32694748215833,2.71063024885284));
#2343=CARTESIAN_POINT('Ctrl Pts',(-1.83766994494307,-2.89448448470946,2.76144202160989));
#2344=CARTESIAN_POINT('Ctrl Pts',(-1.44655561860144,-3.10845518160647,2.78805516977141));
#2345=CARTESIAN_POINT('Ctrl Pts',(-0.600995270357083,-3.37595293922109,
2.84110804243113));
#2346=CARTESIAN_POINT('Ctrl Pts',(-0.15423889345412,-3.42555594121709,2.86585658157997));
#2347=CARTESIAN_POINT('Ctrl Pts',(0.738999393540461,-3.349257097536,2.91716096647369));
#2348=CARTESIAN_POINT('Ctrl Pts',(1.17648243519229,-3.22171906800927,2.94436031210768));
#2349=CARTESIAN_POINT('Ctrl Pts',(1.96233836056712,-2.81053122123338,2.99740286449479));
#2350=CARTESIAN_POINT('Ctrl Pts',(2.30596779573501,-2.53620495219765,3.02166882819812));
#2351=CARTESIAN_POINT('Ctrl Pts',(2.88121057228278,-1.86077478462052,3.0723553044745));
#2352=CARTESIAN_POINT('Ctrl Pts',(3.1025555253124,-1.4621713365509,3.09955334683131));
#2353=CARTESIAN_POINT('Ctrl Pts',(3.34604860374013,-0.697838904257899,3.14754863181823));
#2354=CARTESIAN_POINT('Ctrl Pts',(3.4,-0.349728288913788,3.16809929277934));
#2355=CARTESIAN_POINT('Ctrl Pts',(3.4,4.01761957036229E-13,3.18750000000002));
#2356=CARTESIAN_POINT('Origin',(0.,0.,6.));
#2357=CARTESIAN_POINT('',(3.4,6.57668130322999E-14,4.43750000000001));
#2358=CARTESIAN_POINT('',(3.4,-2.15973304146491E-14,4.4275));
#2359=CARTESIAN_POINT('',(3.4,-4.163799117101E-16,6.));
#2360=CARTESIAN_POINT('',(-1.25288796387014,-3.16073911450935,5.3));
#2361=CARTESIAN_POINT('Ctrl Pts',(3.4,1.3195000597631E-13,4.43750000000001));
#2362=CARTESIAN_POINT('Ctrl Pts',(3.4,0.0484846749858157,4.44018962224077));
#2363=CARTESIAN_POINT('Ctrl Pts',(3.39896290803393,0.0970055128088234,4.44290508080457));
#2364=CARTESIAN_POINT('Ctrl Pts',(3.37748646850743,0.598298156849321,4.47120710147293));
#2365=CARTESIAN_POINT('Ctrl Pts',(3.26776257798046,1.04260348636478,4.49837557212729));
#2366=CARTESIAN_POINT('Ctrl Pts',(2.88783093020024,1.84685112659429,4.55172017709808));
#2367=CARTESIAN_POINT('Ctrl Pts',(2.62723278700067,2.20181240090978,4.57672590475695));
#2368=CARTESIAN_POINT('Ctrl Pts',(1.97369731242403,2.80535577064492,4.62684809170433));
#2369=CARTESIAN_POINT('Ctrl Pts',(1.58253065942841,3.04319173163336,4.65401251725117));
#2370=CARTESIAN_POINT('Ctrl Pts',(0.745875918244429,3.34576782876138,4.70737739133936));
#2371=CARTESIAN_POINT('Ctrl Pts',(0.310730749827996,3.41377166583742,4.7324461843677));
#2372=CARTESIAN_POINT('Ctrl Pts',(-0.578457082509039,3.38097745401162,4.78252622885647));
#2373=CARTESIAN_POINT('Ctrl Pts',(-1.02366424672491,3.27378194584287,4.80968663055877));
#2374=CARTESIAN_POINT('Ctrl Pts',(-1.83045062995484,2.89827699340989,4.86307035254325));
#2375=CARTESIAN_POINT('Ctrl Pts',(-2.18699995734974,2.63959876703994,4.88819955916222));
#2376=CARTESIAN_POINT('Ctrl Pts',(-2.79445461069521,1.98915973325728,4.9382398484591));
#2377=CARTESIAN_POINT('Ctrl Pts',(-3.03456603866918,1.5990797670419,4.96539627706253));
#2378=CARTESIAN_POINT('Ctrl Pts',(-3.34176724206059,0.763685305137532,5.01879751426961));
#2379=CARTESIAN_POINT('Ctrl Pts',(-3.41209993472139,0.328760199170906,5.04398443781417));
#2380=CARTESIAN_POINT('Ctrl Pts',(-3.38395618451195,-0.560962172903048,
5.09398727714361));
#2381=CARTESIAN_POINT('Ctrl Pts',(-3.27899342481953,-1.00695228698157,5.12113980797507));
#2382=CARTESIAN_POINT('Ctrl Pts',(-2.90739622987095,-1.81596630216988,5.17455731262962));
#2383=CARTESIAN_POINT('Ctrl Pts',(-2.65040817232962,-2.17391423643435,5.19979923899294));
#2384=CARTESIAN_POINT('Ctrl Pts',(-2.01958836457687,-2.76887523380191,5.24846409957791));
#2385=CARTESIAN_POINT('Ctrl Pts',(-1.65308929437083,-3.00210298164807,5.27415423684201));
#2386=CARTESIAN_POINT('Ctrl Pts',(-1.25288796387014,-3.16073911450935,5.3));
#2387=CARTESIAN_POINT('',(-1.0964822158325,-3.21834223636379,5.3));
#2388=CARTESIAN_POINT('Origin',(0.,0.,5.3));
#2389=CARTESIAN_POINT('Ctrl Pts',(-1.0964822158325,-3.21834223636379,5.3));
#2390=CARTESIAN_POINT('Ctrl Pts',(-1.45430969353474,-3.09643119122895,5.27734873633288));
#2391=CARTESIAN_POINT('Ctrl Pts',(-1.78932501450223,-2.9156906147822,5.25461116491904));
#2392=CARTESIAN_POINT('Ctrl Pts',(-2.38035325487317,-2.45588612176912,5.21125930631007));
#2393=CARTESIAN_POINT('Ctrl Pts',(-2.63375551357983,-2.18192473180001,5.1911460653954));
#2394=CARTESIAN_POINT('Ctrl Pts',(-3.08389885895375,-1.49967564665538,5.14295584619396));
#2395=CARTESIAN_POINT('Ctrl Pts',(-3.25401415229429,-1.08206016471883,5.11588028889413));
#2396=CARTESIAN_POINT('Ctrl Pts',(-3.42138906401064,-0.213729663558886,
5.06386488944011));
#2397=CARTESIAN_POINT('Ctrl Pts',(-3.4204678818224,0.227997362699221,5.04032246223822));
#2398=CARTESIAN_POINT('Ctrl Pts',(-3.24953923825127,1.0952858313522,4.9882832106968));
#2399=CARTESIAN_POINT('Ctrl Pts',(-3.07788020472564,1.51188914513325,4.96122833009511));
#2400=CARTESIAN_POINT('Ctrl Pts',(-2.58801584204305,2.24812277445386,4.90913068359549));
#2401=CARTESIAN_POINT('Ctrl Pts',(-2.27718857434759,2.56247822644399,4.88556850445372));
#2402=CARTESIAN_POINT('Ctrl Pts',(-1.54680891679612,3.06043075287894,4.83360974982649));
#2403=CARTESIAN_POINT('Ctrl Pts',(-1.1325180731347,3.23670388222288,4.80657712797727));
#2404=CARTESIAN_POINT('Ctrl Pts',(-0.266912011122178,3.41774214395029,4.75439890747381));
#2405=CARTESIAN_POINT('Ctrl Pts',(0.175502624023416,3.42365349401457,4.73080773618714));
#2406=CARTESIAN_POINT('Ctrl Pts',(1.04531165999775,3.26586547764908,4.67893060411707));
#2407=CARTESIAN_POINT('Ctrl Pts',(1.46386269391496,3.10091128189926,4.65192173972419));
#2408=CARTESIAN_POINT('Ctrl Pts',(2.20777213360059,2.62264912216571,4.59966488268835));
#2409=CARTESIAN_POINT('Ctrl Pts',(2.52743823870374,2.31616140221252,4.57603561652486));
#2410=CARTESIAN_POINT('Ctrl Pts',(3.03638972506586,1.59329637088458,4.52424099224271));
#2411=CARTESIAN_POINT('Ctrl Pts',(3.21872315951981,1.18239761726984,4.49725728869968));
#2412=CARTESIAN_POINT('Ctrl Pts',(3.37218516276219,0.501993715429373,4.45598655499202));
#2413=CARTESIAN_POINT('Ctrl Pts',(3.4,0.251114956290832,4.44143026500901));
#2414=CARTESIAN_POINT('Ctrl Pts',(3.4,-4.10088629720917E-14,4.4275));
#2415=CARTESIAN_POINT('Origin',(0.,0.,5.5));
#2416=CARTESIAN_POINT('',(-5.5021444402588,-6.73818357720935E-16,6.));
#2417=CARTESIAN_POINT('Origin',(0.,0.,6.));
#2418=CARTESIAN_POINT('',(-5.73919435177631,-7.02848599258743E-16,5.94023554996109));
#2419=CARTESIAN_POINT('Origin',(-5.5021444402588,-6.73818357720935E-16,
5.5));
#2420=CARTESIAN_POINT('',(5.73919435177631,7.76091229894499E-16,5.94023554996109));
#2421=CARTESIAN_POINT('Origin',(0.,0.,5.94023554996109));
#2422=CARTESIAN_POINT('Origin',(0.,0.,5.94023554996109));
#2423=CARTESIAN_POINT('Origin',(0.,0.,0.5));
#2424=CARTESIAN_POINT('',(-5.73919435177631,-7.02848599258743E-16,0.0597644500389123));
#2425=CARTESIAN_POINT('Origin',(0.,0.,0.0597644500389123));
#2426=CARTESIAN_POINT('',(-5.5021444402588,-6.73818357720935E-16,0.));
#2427=CARTESIAN_POINT('Origin',(-5.5021444402588,-6.73818357720935E-16,
0.5));
#2428=CARTESIAN_POINT('Origin',(0.,0.,0.));
#2429=CARTESIAN_POINT('Origin',(0.,0.,5.5));
#2430=CARTESIAN_POINT('',(-1.78291230217383,-3.52871196543851,5.8535533905933));
#2431=CARTESIAN_POINT('',(-3.95355339059327,-4.84170650504822E-16,5.85355339059327));
#2432=CARTESIAN_POINT('Origin',(0.,0.,5.85355339059327));
#2433=CARTESIAN_POINT('',(-1.92533487773279,-3.50614968428127,5.89456992403025));
#2434=CARTESIAN_POINT('Ctrl Pts',(-1.92533487773279,-3.50614968428128,5.89456992403026));
#2435=CARTESIAN_POINT('Ctrl Pts',(-1.90194360167476,-3.5135341387333,5.89084462065203));
#2436=CARTESIAN_POINT('Ctrl Pts',(-1.87630613215172,-3.52080459320752,5.88625665441102));
#2437=CARTESIAN_POINT('Ctrl Pts',(-1.83861259533635,-3.52885529691004,5.87739687639672));
#2438=CARTESIAN_POINT('Ctrl Pts',(-1.8221693883486,-3.5317119505949,5.87301471768675));
#2439=CARTESIAN_POINT('Ctrl Pts',(-1.8031965360398,-3.5325292633732,5.86571767937469));
#2440=CARTESIAN_POINT('Ctrl Pts',(-1.7978467878905,-3.53246960617574,5.86339641603733));
#2441=CARTESIAN_POINT('Ctrl Pts',(-1.78939267540214,-3.53128566216656,5.85871066493838));
#2442=CARTESIAN_POINT('Ctrl Pts',(-1.78573164524593,-3.53035794931988,5.85629392382858));
#2443=CARTESIAN_POINT('Ctrl Pts',(-1.78291230217384,-3.5287119654385,5.85355339059329));
#2444=CARTESIAN_POINT('',(-3.23003245950903,-2.27979707930028,5.85355339059283));
#2445=CARTESIAN_POINT('Ctrl Pts',(-3.23003245950903,-2.27979707930028,5.85355339059283));
#2446=CARTESIAN_POINT('Ctrl Pts',(-3.06237060858304,-2.53028665703206,5.86101811512799));
#2447=CARTESIAN_POINT('Ctrl Pts',(-2.8672692603167,-2.75973624708032,5.86778388571594));
#2448=CARTESIAN_POINT('Ctrl Pts',(-2.42798671078865,-3.17234364110549,5.88125347566854));
#2449=CARTESIAN_POINT('Ctrl Pts',(-2.18560986572065,-3.35359023328628,5.8879969490314));
#2450=CARTESIAN_POINT('Ctrl Pts',(-1.92533487773279,-3.50614968428127,5.89456992403025));
#2451=CARTESIAN_POINT('Origin',(0.,0.,5.85355339059327));
#2452=CARTESIAN_POINT('',(-4.30710678118655,-5.27468453316596E-16,6.));
#2453=CARTESIAN_POINT('Origin',(-4.30710678118655,-5.27468453316596E-16,
5.5));
#2454=CARTESIAN_POINT('Origin',(0.,0.,6.));
#2455=CARTESIAN_POINT('Origin',(0.,0.,0.5));
#2456=CARTESIAN_POINT('',(-4.30710678118655,-5.27468453316597E-16,0.));
#2457=CARTESIAN_POINT('Origin',(0.,0.,0.));
#2458=CARTESIAN_POINT('',(-3.95355339059327,-4.84170650504822E-16,0.146446609406728));
#2459=CARTESIAN_POINT('Origin',(-4.30710678118655,-5.27468453316597E-16,
0.5));
#2460=CARTESIAN_POINT('',(3.8670348623328,0.822572662914562,0.146446609406718));
#2461=CARTESIAN_POINT('Origin',(0.,0.,0.146446609406727));
#2462=CARTESIAN_POINT('',(3.88127665353657,0.967311500351366,0.105430075969749));
#2463=CARTESIAN_POINT('Ctrl Pts',(3.88127665353656,0.967311500351366,0.105430075969749));
#2464=CARTESIAN_POINT('Ctrl Pts',(3.88248308853003,0.942624045074989,0.109165675612358));
#2465=CARTESIAN_POINT('Ctrl Pts',(3.88301386655303,0.91577332765413,0.11376015133996));
#2466=CARTESIAN_POINT('Ctrl Pts',(3.88125811584264,0.87695729052849,0.122614170727277));
#2467=CARTESIAN_POINT('Ctrl Pts',(3.87986047067845,0.86016035953523,0.12699679547179));
#2468=CARTESIAN_POINT('Ctrl Pts',(3.87585665541296,0.841420755760116,0.134285593835466));
#2469=CARTESIAN_POINT('Ctrl Pts',(3.87444654520301,0.836203179878026,0.136606342515798));
#2470=CARTESIAN_POINT('Ctrl Pts',(3.87116677266274,0.828250561618554,0.141286175182243));
#2471=CARTESIAN_POINT('Ctrl Pts',(3.86934405717525,0.824905655118957,0.143702548179272));
#2472=CARTESIAN_POINT('Ctrl Pts',(3.8670348623328,0.822572662914562,0.14644660940672));
#2473=CARTESIAN_POINT('',(3.06184528645475,2.50113731212209,0.146446609406361));
#2474=CARTESIAN_POINT('Ctrl Pts',(3.06184528645475,2.50113731212209,0.146446609406361));
#2475=CARTESIAN_POINT('Ctrl Pts',(3.25229900237144,2.27922540622542,0.139337140594871));
#2476=CARTESIAN_POINT('Ctrl Pts',(3.4178992421145,2.03712868284477,0.132251957017881));
#2477=CARTESIAN_POINT('Ctrl Pts',(3.69349621819754,1.52125455462991,0.118447746003577));
#2478=CARTESIAN_POINT('Ctrl Pts',(3.80267865496227,1.24900013388164,0.11176958286899));
#2479=CARTESIAN_POINT('Ctrl Pts',(3.88127665353657,0.967311500351366,0.105430075969749));
#2480=CARTESIAN_POINT('Origin',(0.,0.,0.146446609406727));
#2481=CARTESIAN_POINT('Origin',(0.,0.,5.3));
#2482=CARTESIAN_POINT('Ctrl Pts',(-3.23003245950872,-2.27979707930074,5.85355339059284));
#2483=CARTESIAN_POINT('Ctrl Pts',(-3.48605757216865,-1.89729132736786,5.8421545128545));
#2484=CARTESIAN_POINT('Ctrl Pts',(-3.67290272589447,-1.47278615773723,5.83034317876559));
#2485=CARTESIAN_POINT('Ctrl Pts',(-3.90198272549636,-0.534286906649729,
5.80580144893728));
#2486=CARTESIAN_POINT('Ctrl Pts',(-3.92678469732619,-0.02095778682808,5.79389770355618));
#2487=CARTESIAN_POINT('Ctrl Pts',(-3.81417632172746,0.728069662839366,5.77501120790831));
#2488=CARTESIAN_POINT('Ctrl Pts',(-3.7531401911908,0.970805272996208,5.76861936561077));
#2489=CARTESIAN_POINT('Ctrl Pts',(-3.50475866615656,1.66529912267685,5.74950565622732));
#2490=CARTESIAN_POINT('Ctrl Pts',(-3.25470781791685,2.08932025578728,5.73673040142659));
#2491=CARTESIAN_POINT('Ctrl Pts',(-2.76729357820159,2.64262507560001,5.71826865242523));
#2492=CARTESIAN_POINT('Ctrl Pts',(-2.58350558298145,2.81460592309003,5.7122710989614));
#2493=CARTESIAN_POINT('Ctrl Pts',(-2.18871662021604,3.11566208020901,5.69970279956277));
#2494=CARTESIAN_POINT('Ctrl Pts',(-1.97971756236558,3.24500780490607,5.69331974913885));
#2495=CARTESIAN_POINT('Ctrl Pts',(-1.32932365492135,3.5647148010959,5.67419034251822));
#2496=CARTESIAN_POINT('Ctrl Pts',(-0.862609493406725,3.69236352207214,5.66136219147516));
#2497=CARTESIAN_POINT('Ctrl Pts',(-0.141997420183257,3.74802113639565,5.64282043347147));
#2498=CARTESIAN_POINT('Ctrl Pts',(0.103704543707698,3.74343271684464,5.63684833894108));
#2499=CARTESIAN_POINT('Ctrl Pts',(0.808078967993443,3.65931037385989,5.61861265296486));
#2500=CARTESIAN_POINT('Ctrl Pts',(1.25466121318322,3.51794596391685,5.60603376474256));
#2501=CARTESIAN_POINT('Ctrl Pts',(1.87377897388947,3.1843067039061,5.5869756032409));
#2502=CARTESIAN_POINT('Ctrl Pts',(2.07267489777189,3.05081927368397,5.58054440091542));
#2503=CARTESIAN_POINT('Ctrl Pts',(2.62925119655528,2.59340895698975,5.56157229450649));
#2504=CARTESIAN_POINT('Ctrl Pts',(2.93852342211069,2.21760690130707,5.54955345539839));
#2505=CARTESIAN_POINT('Ctrl Pts',(3.38505687577488,1.37528752962112,5.52343629412718));
#2506=CARTESIAN_POINT('Ctrl Pts',(3.52229264131942,0.921136157090413,5.51030337752685));
#2507=CARTESIAN_POINT('Ctrl Pts',(3.61579848004809,-0.0158981524309145,
5.48495880691041));
#2508=CARTESIAN_POINT('Ctrl Pts',(3.57061186396643,-0.490757310244434,5.47293902065656));
#2509=CARTESIAN_POINT('Ctrl Pts',(3.29802269785456,-1.38356055051093,5.44682324267042));
#2510=CARTESIAN_POINT('Ctrl Pts',(3.07950407722148,-1.793017386471,5.43369601743825));
#2511=CARTESIAN_POINT('Ctrl Pts',(2.49700735160396,-2.50729774012675,5.40833391065028));
#2512=CARTESIAN_POINT('Ctrl Pts',(2.13732363548428,-2.80556135170051,5.39631287055879));
#2513=CARTESIAN_POINT('Ctrl Pts',(1.33146390865158,-3.23596187835134,5.37019862528225));
#2514=CARTESIAN_POINT('Ctrl Pts',(0.897477746127028,-3.36866325812721,5.35707701665436));
#2515=CARTESIAN_POINT('Ctrl Pts',(0.184867188647294,-3.44228476569018,5.33691297012429));
#2516=CARTESIAN_POINT('Ctrl Pts',(-0.0852040363592367,-3.43924476673309,
5.32978546915416));
#2517=CARTESIAN_POINT('Ctrl Pts',(-0.606244419702814,-3.37055296824439,
5.31501529318569));
#2518=CARTESIAN_POINT('Ctrl Pts',(-0.856073829920963,-3.30823594612872,
5.30756035389141));
#2519=CARTESIAN_POINT('Ctrl Pts',(-1.09648221583289,-3.21834223636364,5.29999999999999));
#2520=CARTESIAN_POINT('Ctrl Pts',(-1.78291230217383,-3.52871196543852,5.85355339059329));
#2521=CARTESIAN_POINT('Ctrl Pts',(-1.65032523775131,-3.45130522020063,5.72467256717835));
#2522=CARTESIAN_POINT('Ctrl Pts',(-1.52284260312185,-3.36708660390191,5.59465869876949));
#2523=CARTESIAN_POINT('Ctrl Pts',(-1.40116082960876,-3.27654653614685,5.46356687519203));
#2524=CARTESIAN_POINT('Ctrl Pts',(-1.35072296474922,-3.23901710532119,5.40922848505441));
#2525=CARTESIAN_POINT('Ctrl Pts',(-1.30128192586066,-3.20040211538145,5.35470488551682));
#2526=CARTESIAN_POINT('Ctrl Pts',(-1.25288796387014,-3.16073911450935,5.3));
#2527=CARTESIAN_POINT('Origin',(0.,0.,0.));
#2528=CARTESIAN_POINT('Ctrl Pts',(3.06184528645506,2.50113731212173,0.146446609406349));
#2529=CARTESIAN_POINT('Ctrl Pts',(2.77435240222989,2.8361168296548,0.15717846456648));
#2530=CARTESIAN_POINT('Ctrl Pts',(2.43294573365056,3.12119414411317,0.167440655963785));
#2531=CARTESIAN_POINT('Ctrl Pts',(1.6853369919954,3.5539312966052,0.189277673693473));
#2532=CARTESIAN_POINT('Ctrl Pts',(1.28936104917625,3.70449697040217,0.200164930942241));
#2533=CARTESIAN_POINT('Ctrl Pts',(0.414742223530389,3.88361747138701,0.222891527846362));
#2534=CARTESIAN_POINT('Ctrl Pts',(-0.102681428720145,3.90226753828496,0.234832426921827));
#2535=CARTESIAN_POINT('Ctrl Pts',(-1.1281484694038,3.70272941302675,0.261366829194983));
#2536=CARTESIAN_POINT('Ctrl Pts',(-1.59371735193676,3.51313738339041,0.274524268420465));
#2537=CARTESIAN_POINT('Ctrl Pts',(-2.39606359536181,2.98601592969997,0.299463936486715));
#2538=CARTESIAN_POINT('Ctrl Pts',(-2.76812379329783,2.64148334326332,0.311401996056597));
#2539=CARTESIAN_POINT('Ctrl Pts',(-3.20456765415488,1.9976794673569,0.331543524760906));
#2540=CARTESIAN_POINT('Ctrl Pts',(-3.32080929617615,1.78433802431732,0.337962163790949));
#2541=CARTESIAN_POINT('Ctrl Pts',(-3.60018016321903,1.12728340083744,0.357030647934769));
#2542=CARTESIAN_POINT('Ctrl Pts',(-3.70120939598955,0.66235242669122,0.369666669227658));
#2543=CARTESIAN_POINT('Ctrl Pts',(-3.71971832458559,-0.0514672817840994,
0.387829343601874));
#2544=CARTESIAN_POINT('Ctrl Pts',(-3.70248187722653,-0.293585158448379,
0.393850398705496));
#2545=CARTESIAN_POINT('Ctrl Pts',(-3.5819983306588,-0.991762845935543,0.41248195793184));
#2546=CARTESIAN_POINT('Ctrl Pts',(-3.41639083385021,-1.43124925906229,0.42526125755466));
#2547=CARTESIAN_POINT('Ctrl Pts',(-2.9216272443319,-2.23850002061275,0.450991006289752));
#2548=CARTESIAN_POINT('Ctrl Pts',(-2.58993108590179,-2.59866365023318,0.463093178436547));
#2549=CARTESIAN_POINT('Ctrl Pts',(-1.8288152789984,-3.14755490593119,0.488216083183662));
#2550=CARTESIAN_POINT('Ctrl Pts',(-1.41283102553677,-3.3412129182102,0.500953731458646));
#2551=CARTESIAN_POINT('Ctrl Pts',(-0.514426264589624,-3.56737174753317,
0.526698120079665));
#2552=CARTESIAN_POINT('Ctrl Pts',(-0.035457866608088,-3.59227952289105,
0.5388576269144));
#2553=CARTESIAN_POINT('Ctrl Pts',(0.871840240219401,-3.45560228292562,0.563867472849291));
#2554=CARTESIAN_POINT('Ctrl Pts',(1.29449180806901,-3.30695688143785,0.57655861188009));
#2555=CARTESIAN_POINT('Ctrl Pts',(1.87507805263777,-2.96922557851636,0.595651996080249));
#2556=CARTESIAN_POINT('Ctrl Pts',(2.06025795852984,-2.83596564228176,0.602058454826432));
#2557=CARTESIAN_POINT('Ctrl Pts',(2.40416549124293,-2.53391662692938,0.614625275375867));
#2558=CARTESIAN_POINT('Ctrl Pts',(2.56306026431644,-2.36433530990857,0.620688671243676));
#2559=CARTESIAN_POINT('Ctrl Pts',(2.96597110497598,-1.8352358126166,0.639127980815));
#2560=CARTESIAN_POINT('Ctrl Pts',(3.16100735459105,-1.44424233619295,0.651755137766466));
#2561=CARTESIAN_POINT('Ctrl Pts',(3.33449176366876,-0.828384328578818,0.670371247269878));
#2562=CARTESIAN_POINT('Ctrl Pts',(3.37251101126901,-0.624749332251278,0.676341748573088));
#2563=CARTESIAN_POINT('Ctrl Pts',(3.41216803127686,-0.206693409248142,0.688226656305019));
#2564=CARTESIAN_POINT('Ctrl Pts',(3.41272231692649,0.00880057830198792,
0.694005688511974));
#2565=CARTESIAN_POINT('Ctrl Pts',(3.39272377138046,0.222318265353878,0.700000000000002));
#2566=CARTESIAN_POINT('Ctrl Pts',(3.8670348623328,0.822572662914563,0.146446609406718));
#2567=CARTESIAN_POINT('Ctrl Pts',(3.77302895909947,0.727597983697717,0.25815565598544));
#2568=CARTESIAN_POINT('Ctrl Pts',(3.67519496548545,0.637291809812134,0.370594064843146));
#2569=CARTESIAN_POINT('Ctrl Pts',(3.5738640727637,0.552046912101368,0.483750533529002));
#2570=CARTESIAN_POINT('Ctrl Pts',(3.50957206027576,0.497961076272375,0.555545589335125));
#2571=CARTESIAN_POINT('Ctrl Pts',(3.44387284612637,0.445913479209334,0.627629707095193));
#2572=CARTESIAN_POINT('Ctrl Pts',(3.37685862035149,0.396012446973337,0.700000000000002));
#2573=CARTESIAN_POINT('Origin',(0.,0.,0.));
#2574=CARTESIAN_POINT('',(3.46410161513774,-6.,0.700000000000016));
#2575=CARTESIAN_POINT('',(6.92820323027547,-5.50774703622636E-14,0.7));
#2576=CARTESIAN_POINT('Ctrl Pts',(3.46410161513143,-6.00000000001093,0.700000000003416));
#2577=CARTESIAN_POINT('Ctrl Pts',(5.19615242270661,-3.00000000000003,-0.232642742539615));
#2578=CARTESIAN_POINT('Ctrl Pts',(6.92820323028178,1.08718214755315E-11,
0.700000000003399));
#2579=CARTESIAN_POINT('',(-3.46410161513767,-6.00000000000001,0.7));
#2580=CARTESIAN_POINT('Ctrl Pts',(-3.46410161515028,-6.00000000000001,0.700000000003395));
#2581=CARTESIAN_POINT('Ctrl Pts',(3.30846461338297E-14,-6.,-0.232642742539606));
#2582=CARTESIAN_POINT('Ctrl Pts',(3.46410161515036,-6.,0.700000000003413));
#2583=CARTESIAN_POINT('',(-6.92820323027547,-1.26634813746307E-13,0.7));
#2584=CARTESIAN_POINT('Ctrl Pts',(-6.92820323028178,1.07991580485185E-11,
0.700000000003397));
#2585=CARTESIAN_POINT('Ctrl Pts',(-5.19615242270662,-3.00000000000007,-0.23264274253959));
#2586=CARTESIAN_POINT('Ctrl Pts',(-3.46410161513145,-6.00000000001097,0.700000000003437));
#2587=CARTESIAN_POINT('',(-5.62820323027547,-6.89256107090765E-16,0.));
#2588=CARTESIAN_POINT('',(-3.46410161513784,5.99999999999991,0.7));
#2589=CARTESIAN_POINT('Ctrl Pts',(-3.46410161513153,6.00000000001084,0.700000000003399));
#2590=CARTESIAN_POINT('Ctrl Pts',(-5.19615242270669,2.99999999999995,-0.232642742539597));
#2591=CARTESIAN_POINT('Ctrl Pts',(-6.92820323028188,-1.09821184038314E-11,
0.70000000000345));
#2592=CARTESIAN_POINT('',(3.46410161513769,6.,0.7));
#2593=CARTESIAN_POINT('Ctrl Pts',(3.46410161515031,6.,0.700000000003399));
#2594=CARTESIAN_POINT('Ctrl Pts',(-4.9960036108132E-14,6.,-0.232642742539617));
#2595=CARTESIAN_POINT('Ctrl Pts',(-3.46410161515044,6.,0.700000000003435));
#2596=CARTESIAN_POINT('Ctrl Pts',(6.92820323028178,-1.09842486020173E-11,
0.700000000003399));
#2597=CARTESIAN_POINT('Ctrl Pts',(5.19615242270659,2.99999999999997,-0.232642742539654));
#2598=CARTESIAN_POINT('Ctrl Pts',(3.46410161513139,6.00000000001092,0.700000000003399));
#2599=CARTESIAN_POINT('Origin',(0.,0.,5.3));
#2600=CARTESIAN_POINT('',(-3.46410161513778,-6.00000000000001,5.29999999999997));
#2601=CARTESIAN_POINT('',(-6.92820323027547,-1.26634813746307E-13,5.3));
#2602=CARTESIAN_POINT('Ctrl Pts',(-3.46410161512789,-6.00000000001713,5.29999999999465));
#2603=CARTESIAN_POINT('Ctrl Pts',(-5.19615242270664,-3.00000000000005,6.23264274254104));
#2604=CARTESIAN_POINT('Ctrl Pts',(-6.92820323028537,1.70112774321325E-11,
5.29999999999467));
#2605=CARTESIAN_POINT('',(3.46410161513769,-6.,5.3));
#2606=CARTESIAN_POINT('Ctrl Pts',(3.46410161515748,-6.,5.29999999999467));
#2607=CARTESIAN_POINT('Ctrl Pts',(-3.06421554796543E-14,-6.,6.23264274254106));
#2608=CARTESIAN_POINT('Ctrl Pts',(-3.46410161515757,-6.,5.29999999999464));
#2609=CARTESIAN_POINT('',(6.92820323027547,-5.50774703622636E-14,5.3));
#2610=CARTESIAN_POINT('Ctrl Pts',(6.92820323028536,1.70703849372499E-11,
5.29999999999468));
#2611=CARTESIAN_POINT('Ctrl Pts',(5.19615242270661,-3.00000000000003,6.23264274254106));
#2612=CARTESIAN_POINT('Ctrl Pts',(3.46410161512784,-6.00000000001715,5.29999999999465));
#2613=CARTESIAN_POINT('',(6.92820323027547,-8.48460190979921E-16,5.3));
#2614=CARTESIAN_POINT('',(3.46410161513769,6.,5.3));
#2615=CARTESIAN_POINT('Ctrl Pts',(3.4641016151278,6.00000000001713,5.29999999999467));
#2616=CARTESIAN_POINT('Ctrl Pts',(5.19615242270659,2.99999999999997,6.2326427425411));
#2617=CARTESIAN_POINT('Ctrl Pts',(6.92820323028537,-1.72005130880512E-11,
5.29999999999467));
#2618=CARTESIAN_POINT('',(-3.46410161513784,5.99999999999991,5.3));
#2619=CARTESIAN_POINT('Ctrl Pts',(-3.46410161515761,6.,5.29999999999464));
#2620=CARTESIAN_POINT('Ctrl Pts',(-4.9737991503207E-14,6.,6.23264274254107));
#2621=CARTESIAN_POINT('Ctrl Pts',(3.46410161515748,6.,5.29999999999467));
#2622=CARTESIAN_POINT('Ctrl Pts',(-6.92820323028547,-1.71902036394844E-11,
5.29999999999462));
#2623=CARTESIAN_POINT('Ctrl Pts',(-5.19615242270669,2.99999999999995,6.23264274254104));
#2624=CARTESIAN_POINT('Ctrl Pts',(-3.46410161512795,6.00000000001704,5.29999999999467));
#2625=CARTESIAN_POINT('Origin',(0.,0.,6.));
#2626=CARTESIAN_POINT('Ctrl Pts',(3.4,-4.1286418728248E-14,4.4275));
#2627=CARTESIAN_POINT('Ctrl Pts',(3.4,-0.186121573168501,4.41717515564813));
#2628=CARTESIAN_POINT('Ctrl Pts',(3.38471908137672,-0.372333688940097,4.40649416451766));
#2629=CARTESIAN_POINT('Ctrl Pts',(3.28124216860171,-0.995696340847217,4.36953627202487));
#2630=CARTESIAN_POINT('Ctrl Pts',(3.12293048658518,-1.41606837879289,4.34257902116854));
#2631=CARTESIAN_POINT('Ctrl Pts',(2.65619550095441,-2.16746765440165,4.2901715462705));
#2632=CARTESIAN_POINT('Ctrl Pts',(2.35399859648627,-2.49238497036037,4.26644003600835));
#2633=CARTESIAN_POINT('Ctrl Pts',(1.63859104158029,-3.01209070895768,4.21481199464172));
#2634=CARTESIAN_POINT('Ctrl Pts',(1.23110761644009,-3.20031628743618,4.18788236252099));
#2635=CARTESIAN_POINT('Ctrl Pts',(0.371201765949229,-3.40821037856945,4.13540326192926));
#2636=CARTESIAN_POINT('Ctrl Pts',(-0.0725687904280879,-3.42759737449122,
4.11160847464233));
#2637=CARTESIAN_POINT('Ctrl Pts',(-0.94703531002039,-3.29552875407992,4.06006395368984));
#2638=CARTESIAN_POINT('Ctrl Pts',(-1.36908596543482,-3.14371830215661,4.0331629686661));
#2639=CARTESIAN_POINT('Ctrl Pts',(-2.12770774344354,-2.688300844554,3.98061488863892));
#2640=CARTESIAN_POINT('Ctrl Pts',(-2.45775731231282,-2.39029937611201,3.95674944530396));
#2641=CARTESIAN_POINT('Ctrl Pts',(-2.98785764954916,-1.68220467166189,3.90528822802077));
#2642=CARTESIAN_POINT('Ctrl Pts',(-3.18174475294303,-1.27811503245704,3.87841677143123));
#2643=CARTESIAN_POINT('Ctrl Pts',(-3.40252747310172,-0.421110543648273,
3.82580246582334));
#2644=CARTESIAN_POINT('Ctrl Pts',(-3.4284082411663,0.0233109517265578,3.8018596191488));
#2645=CARTESIAN_POINT('Ctrl Pts',(-3.30863368964708,0.899875278664372,3.75048121754253));
#2646=CARTESIAN_POINT('Ctrl Pts',(-3.16311132282504,1.32345283364206,3.72364001706537));
#2647=CARTESIAN_POINT('Ctrl Pts',(-2.71867737003119,2.08896069354698,3.67096231921887));
#2648=CARTESIAN_POINT('Ctrl Pts',(-2.42473352762095,2.42396950470071,3.64693600787735));
#2649=CARTESIAN_POINT('Ctrl Pts',(-1.72372676814348,2.96400603940907,3.59563967146296));
#2650=CARTESIAN_POINT('Ctrl Pts',(-1.32296629343995,3.16327215273327,3.56882929723005));
#2651=CARTESIAN_POINT('Ctrl Pts',(-0.468845437377404,3.39640865728536,3.51609109274558));
#2652=CARTESIAN_POINT('Ctrl Pts',(-0.0238015395680562,3.42853269676147,
3.49197598107518));
#2653=CARTESIAN_POINT('Ctrl Pts',(0.854691311762255,3.3205134009099,3.44076070874106));
#2654=CARTESIAN_POINT('Ctrl Pts',(1.27964077780986,3.18100414093045,3.41398157215478));
#2655=CARTESIAN_POINT('Ctrl Pts',(2.05164359087632,2.74711062423187,3.36118577302349));
#2656=CARTESIAN_POINT('Ctrl Pts',(2.39139213819153,2.45704990197379,3.33697727616224));
#2657=CARTESIAN_POINT('Ctrl Pts',(2.94082692627242,1.76283634079008,3.2858418307883));
#2658=CARTESIAN_POINT('Ctrl Pts',(3.14514957850475,1.36530114858836,3.25909418591775));
#2659=CARTESIAN_POINT('Ctrl Pts',(3.35557986947541,0.633683454545388,3.21367342189199));
#2660=CARTESIAN_POINT('Ctrl Pts',(3.40000000000004,0.317340779883098,3.19510405364632));
#2661=CARTESIAN_POINT('Ctrl Pts',(3.4,-4.57203719328447E-13,3.17749999999997));
#2662=CARTESIAN_POINT('Ctrl Pts',(3.4,4.02367417807767E-13,3.18750000000002));
#2663=CARTESIAN_POINT('Ctrl Pts',(3.4,0.084778075557853,3.19220294990359));
#2664=CARTESIAN_POINT('Ctrl Pts',(3.39682921836388,0.169643165693244,3.19698358485793));
#2665=CARTESIAN_POINT('Ctrl Pts',(3.35666479179104,0.704885329940955,3.22759832104023));
#2666=CARTESIAN_POINT('Ctrl Pts',(3.23342729542556,1.14409166058361,3.25479444641897));
#2667=CARTESIAN_POINT('Ctrl Pts',(2.82979832555493,1.93447068967886,3.30791422448257));
#2668=CARTESIAN_POINT('Ctrl Pts',(2.55882097173626,2.2808604668407,3.33233732015604));
#2669=CARTESIAN_POINT('Ctrl Pts',(1.888689857903,2.86305918557583,3.38288967177184));
#2670=CARTESIAN_POINT('Ctrl Pts',(1.49184515045318,3.0884605724715,3.41008335885311));
#2671=CARTESIAN_POINT('Ctrl Pts',(0.648567420366776,3.36590927212086,3.46323825849629));
#2672=CARTESIAN_POINT('Ctrl Pts',(0.212215696658642,3.42124204383506,3.48773952075238));
#2673=CARTESIAN_POINT('Ctrl Pts',(-0.673844997879645,3.36309030641018,3.5382287552024));
#2674=CARTESIAN_POINT('Ctrl Pts',(-1.11458071880527,3.24377623285994,3.56541956927481));
#2675=CARTESIAN_POINT('Ctrl Pts',(-1.90903929904592,2.84703508925413,3.61860738689352));
#2676=CARTESIAN_POINT('Ctrl Pts',(-2.25793303097117,2.57909280652053,3.64318594206919));
#2677=CARTESIAN_POINT('Ctrl Pts',(-2.84640735314467,1.91378832788541,3.69361474302511));
#2678=CARTESIAN_POINT('Ctrl Pts',(-3.07546706131234,1.5185689169317,3.72080232965667));
#2679=CARTESIAN_POINT('Ctrl Pts',(-3.36028375995725,0.677194277000098,3.77402095937644));
#2680=CARTESIAN_POINT('Ctrl Pts',(-3.41933581790506,0.241198415149406,3.79867554450871));
#2681=CARTESIAN_POINT('Ctrl Pts',(-3.36863576566522,-0.645818691105451,
3.84904661023061));
#2682=CARTESIAN_POINT('Ctrl Pts',(-3.25287263204456,-1.08790383774031,3.87623068859344));
#2683=CARTESIAN_POINT('Ctrl Pts',(-2.86235949762462,-1.88601685512811,3.92947812437708));
#2684=CARTESIAN_POINT('Ctrl Pts',(-2.59714842325084,-2.23716566450476,3.95420713965067));
#2685=CARTESIAN_POINT('Ctrl Pts',(-1.93620626854934,-2.83126355461424,4.00452316455724));
#2686=CARTESIAN_POINT('Ctrl Pts',(-1.54247446483059,-3.06359998871188,4.03170352059063));
#2687=CARTESIAN_POINT('Ctrl Pts',(-0.702836250273089,-3.35503314843299,
4.08497785709781));
#2688=CARTESIAN_POINT('Ctrl Pts',(-0.267158441261753,-3.41742225278365,
4.10977941670543));
#2689=CARTESIAN_POINT('Ctrl Pts',(0.620689477376828,-3.37340234046731,4.16004307476651));
#2690=CARTESIAN_POINT('Ctrl Pts',(1.06395928212342,-3.26082992394206,4.18721955433763));
#2691=CARTESIAN_POINT('Ctrl Pts',(1.86532592317619,-2.87590884056273,4.24051898670533));
#2692=CARTESIAN_POINT('Ctrl Pts',(2.21849244667218,-2.61313980059034,4.26539096736468));
#2693=CARTESIAN_POINT('Ctrl Pts',(2.81759901065795,-1.95611272799177,4.31560489736237));
#2694=CARTESIAN_POINT('Ctrl Pts',(3.05285241159819,-1.5637307492961,4.34277739955764));
#2695=CARTESIAN_POINT('Ctrl Pts',(3.33394599822532,-0.771448153098491,4.39318716462197));
#2696=CARTESIAN_POINT('Ctrl Pts',(3.4,-0.386958995796732,4.41603396930755));
#2697=CARTESIAN_POINT('Ctrl Pts',(3.4,1.31769595235198E-13,4.43750000000001));
#2698=CARTESIAN_POINT('Origin',(0.,0.,6.));
#2699=CARTESIAN_POINT('Origin',(0.,0.,0.));
#2700=CARTESIAN_POINT('Origin',(3.46410161513774,-6.,6.));
#2701=CARTESIAN_POINT('',(3.46410161513774,-6.,6.));
#2702=CARTESIAN_POINT('',(6.92820323027547,-5.54031299473484E-14,6.));
#2703=CARTESIAN_POINT('Origin',(6.92820323027547,-5.54031299473484E-14,
6.));
#2704=CARTESIAN_POINT('',(3.4641016151377,6.,6.));
#2705=CARTESIAN_POINT('Origin',(3.4641016151377,6.,6.));
#2706=CARTESIAN_POINT('',(-3.46410161513779,6.,6.));
#2707=CARTESIAN_POINT('Origin',(-3.46410161513779,6.,6.));
#2708=CARTESIAN_POINT('',(-6.92820323027554,-6.46958707310266E-15,6.));
#2709=CARTESIAN_POINT('Origin',(-6.92820323027554,-6.46958707310266E-15,
6.));
#2710=CARTESIAN_POINT('',(-3.46410161513778,-6.00000000000001,6.));
#2711=CARTESIAN_POINT('Origin',(-3.46410161513778,-6.00000000000001,6.));
#2712=CARTESIAN_POINT('Ctrl Pts',(0.,3.4,6.));
#2713=CARTESIAN_POINT('Ctrl Pts',(1.40832611206852,3.4,5.921875));
#2714=CARTESIAN_POINT('Ctrl Pts',(2.40416305603426,2.40416305603426,5.84375));
#2715=CARTESIAN_POINT('Ctrl Pts',(3.4,1.40832611206852,5.765625));
#2716=CARTESIAN_POINT('Ctrl Pts',(3.4,2.0818995585505E-16,5.6875));
#2717=CARTESIAN_POINT('Ctrl Pts',(3.4,-1.40832611206852,5.609375));
#2718=CARTESIAN_POINT('Ctrl Pts',(2.40416305603426,-2.40416305603426,5.53125));
#2719=CARTESIAN_POINT('Ctrl Pts',(1.40832611206852,-3.4,5.453125));
#2720=CARTESIAN_POINT('Ctrl Pts',(4.163799117101E-16,-3.4,5.375));
#2721=CARTESIAN_POINT('Ctrl Pts',(-1.40832611206852,-3.4,5.296875));
#2722=CARTESIAN_POINT('Ctrl Pts',(-2.40416305603426,-2.40416305603426,5.21875));
#2723=CARTESIAN_POINT('Ctrl Pts',(-3.4,-1.40832611206853,5.140625));
#2724=CARTESIAN_POINT('Ctrl Pts',(-3.4,-6.2456986756515E-16,5.0625));
#2725=CARTESIAN_POINT('Ctrl Pts',(-3.4,1.40832611206852,4.984375));
#2726=CARTESIAN_POINT('Ctrl Pts',(-2.40416305603426,2.40416305603426,4.90625));
#2727=CARTESIAN_POINT('Ctrl Pts',(-1.40832611206853,3.4,4.828125));
#2728=CARTESIAN_POINT('Ctrl Pts',(0.,3.4,4.75));
#2729=CARTESIAN_POINT('Ctrl Pts',(1.40832611206852,3.4,4.671875));
#2730=CARTESIAN_POINT('Ctrl Pts',(2.40416305603426,2.40416305603426,4.59375));
#2731=CARTESIAN_POINT('Ctrl Pts',(3.4,1.40832611206852,4.515625));
#2732=CARTESIAN_POINT('Ctrl Pts',(3.4,2.0818995585505E-16,4.4375));
#2733=CARTESIAN_POINT('Ctrl Pts',(3.4,-1.40832611206852,4.359375));
#2734=CARTESIAN_POINT('Ctrl Pts',(2.40416305603426,-2.40416305603426,4.28125));
#2735=CARTESIAN_POINT('Ctrl Pts',(1.40832611206852,-3.4,4.203125));
#2736=CARTESIAN_POINT('Ctrl Pts',(4.163799117101E-16,-3.4,4.125));
#2737=CARTESIAN_POINT('Ctrl Pts',(-1.40832611206852,-3.4,4.046875));
#2738=CARTESIAN_POINT('Ctrl Pts',(-2.40416305603426,-2.40416305603426,3.96875));
#2739=CARTESIAN_POINT('Ctrl Pts',(-3.4,-1.40832611206853,3.890625));
#2740=CARTESIAN_POINT('Ctrl Pts',(-3.4,-6.2456986756515E-16,3.8125));
#2741=CARTESIAN_POINT('Ctrl Pts',(-3.4,1.40832611206852,3.734375));
#2742=CARTESIAN_POINT('Ctrl Pts',(-2.40416305603426,2.40416305603426,3.65625));
#2743=CARTESIAN_POINT('Ctrl Pts',(-1.40832611206853,3.4,3.578125));
#2744=CARTESIAN_POINT('Ctrl Pts',(0.,3.4,3.5));
#2745=CARTESIAN_POINT('Ctrl Pts',(1.40832611206852,3.4,3.421875));
#2746=CARTESIAN_POINT('Ctrl Pts',(2.40416305603426,2.40416305603426,3.34375));
#2747=CARTESIAN_POINT('Ctrl Pts',(3.4,1.40832611206852,3.265625));
#2748=CARTESIAN_POINT('Ctrl Pts',(3.4,2.0818995585505E-16,3.1875));
#2749=CARTESIAN_POINT('Ctrl Pts',(3.4,-1.40832611206852,3.109375));
#2750=CARTESIAN_POINT('Ctrl Pts',(2.40416305603426,-2.40416305603426,3.03125));
#2751=CARTESIAN_POINT('Ctrl Pts',(1.40832611206852,-3.4,2.953125));
#2752=CARTESIAN_POINT('Ctrl Pts',(4.163799117101E-16,-3.4,2.875));
#2753=CARTESIAN_POINT('Ctrl Pts',(-1.40832611206852,-3.4,2.796875));
#2754=CARTESIAN_POINT('Ctrl Pts',(-2.40416305603426,-2.40416305603426,2.71875));
#2755=CARTESIAN_POINT('Ctrl Pts',(-3.4,-1.40832611206853,2.640625));
#2756=CARTESIAN_POINT('Ctrl Pts',(-3.4,-6.2456986756515E-16,2.5625));
#2757=CARTESIAN_POINT('Ctrl Pts',(-3.4,1.40832611206852,2.484375));
#2758=CARTESIAN_POINT('Ctrl Pts',(-2.40416305603426,2.40416305603426,2.40625));
#2759=CARTESIAN_POINT('Ctrl Pts',(-1.40832611206853,3.4,2.328125));
#2760=CARTESIAN_POINT('Ctrl Pts',(0.,3.4,2.25));
#2761=CARTESIAN_POINT('Ctrl Pts',(1.40832611206852,3.4,2.171875));
#2762=CARTESIAN_POINT('Ctrl Pts',(2.40416305603426,2.40416305603426,2.09375));
#2763=CARTESIAN_POINT('Ctrl Pts',(3.4,1.40832611206852,2.015625));
#2764=CARTESIAN_POINT('Ctrl Pts',(3.4,2.0818995585505E-16,1.9375));
#2765=CARTESIAN_POINT('Ctrl Pts',(3.4,-1.40832611206852,1.859375));
#2766=CARTESIAN_POINT('Ctrl Pts',(2.40416305603426,-2.40416305603426,1.78125));
#2767=CARTESIAN_POINT('Ctrl Pts',(1.40832611206852,-3.4,1.703125));
#2768=CARTESIAN_POINT('Ctrl Pts',(4.163799117101E-16,-3.4,1.625));
#2769=CARTESIAN_POINT('Ctrl Pts',(-1.40832611206852,-3.4,1.546875));
#2770=CARTESIAN_POINT('Ctrl Pts',(-2.40416305603426,-2.40416305603426,1.46875));
#2771=CARTESIAN_POINT('Ctrl Pts',(-3.4,-1.40832611206853,1.390625));
#2772=CARTESIAN_POINT('Ctrl Pts',(-3.4,-6.2456986756515E-16,1.3125));
#2773=CARTESIAN_POINT('Ctrl Pts',(-3.4,1.40832611206852,1.234375));
#2774=CARTESIAN_POINT('Ctrl Pts',(-2.40416305603426,2.40416305603426,1.15625));
#2775=CARTESIAN_POINT('Ctrl Pts',(-1.40832611206853,3.4,1.078125));
#2776=CARTESIAN_POINT('Ctrl Pts',(0.,3.4,1.));
#2777=CARTESIAN_POINT('Ctrl Pts',(1.40832611206852,3.4,0.921875));
#2778=CARTESIAN_POINT('Ctrl Pts',(2.40416305603426,2.40416305603426,0.84375));
#2779=CARTESIAN_POINT('Ctrl Pts',(3.4,1.40832611206852,0.765625));
#2780=CARTESIAN_POINT('Ctrl Pts',(3.4,2.0818995585505E-16,0.6875));
#2781=CARTESIAN_POINT('Ctrl Pts',(3.4,-1.40832611206852,0.609375));
#2782=CARTESIAN_POINT('Ctrl Pts',(2.40416305603426,-2.40416305603426,0.53125));
#2783=CARTESIAN_POINT('Ctrl Pts',(1.40832611206852,-3.4,0.453125));
#2784=CARTESIAN_POINT('Ctrl Pts',(4.163799117101E-16,-3.4,0.375));
#2785=CARTESIAN_POINT('Ctrl Pts',(-1.40832611206852,-3.4,0.296875));
#2786=CARTESIAN_POINT('Ctrl Pts',(-2.40416305603426,-2.40416305603426,0.21875));
#2787=CARTESIAN_POINT('Ctrl Pts',(-3.4,-1.40832611206853,0.140625));
#2788=CARTESIAN_POINT('Ctrl Pts',(-3.4,-6.2456986756515E-16,0.0625000000000001));
#2789=CARTESIAN_POINT('Ctrl Pts',(-3.4,1.40832611206852,-0.015625));
#2790=CARTESIAN_POINT('Ctrl Pts',(-2.40416305603426,2.40416305603426,-0.0937500000000001));
#2791=CARTESIAN_POINT('Ctrl Pts',(-1.40832611206853,3.4,-0.171875));
#2792=CARTESIAN_POINT('Ctrl Pts',(0.,3.4,-0.25));
#2793=CARTESIAN_POINT('Ctrl Pts',(1.40832611206852,3.4,-0.328125));
#2794=CARTESIAN_POINT('Ctrl Pts',(2.40416305603426,2.40416305603426,-0.40625));
#2795=CARTESIAN_POINT('Ctrl Pts',(3.4,1.40832611206852,-0.484375));
#2796=CARTESIAN_POINT('Ctrl Pts',(3.4,2.0818995585505E-16,-0.5625));
#2797=CARTESIAN_POINT('Ctrl Pts',(3.4,-1.40832611206852,-0.640625));
#2798=CARTESIAN_POINT('Ctrl Pts',(2.40416305603426,-2.40416305603426,-0.71875));
#2799=CARTESIAN_POINT('Ctrl Pts',(1.40832611206852,-3.4,-0.796875));
#2800=CARTESIAN_POINT('Ctrl Pts',(4.163799117101E-16,-3.4,-0.875));
#2801=CARTESIAN_POINT('Ctrl Pts',(-1.40832611206852,-3.4,-0.953125));
#2802=CARTESIAN_POINT('Ctrl Pts',(-2.40416305603426,-2.40416305603426,-1.03125));
#2803=CARTESIAN_POINT('Ctrl Pts',(-3.4,-1.40832611206853,-1.109375));
#2804=CARTESIAN_POINT('Ctrl Pts',(-3.4,-6.2456986756515E-16,-1.1875));
#2805=CARTESIAN_POINT('Ctrl Pts',(-3.4,1.40832611206852,-1.265625));
#2806=CARTESIAN_POINT('Ctrl Pts',(-2.40416305603426,2.40416305603426,-1.34375));
#2807=CARTESIAN_POINT('Ctrl Pts',(-1.40832611206853,3.4,-1.421875));
#2808=CARTESIAN_POINT('Ctrl Pts',(0.,3.4,-1.5));
#2809=CARTESIAN_POINT('Ctrl Pts',(0.,4.,6.62));
#2810=CARTESIAN_POINT('Ctrl Pts',(1.65685424949238,4.,6.541875));
#2811=CARTESIAN_POINT('Ctrl Pts',(2.82842712474619,2.82842712474619,6.46375));
#2812=CARTESIAN_POINT('Ctrl Pts',(4.,1.65685424949238,6.385625));
#2813=CARTESIAN_POINT('Ctrl Pts',(4.,2.44929359829471E-16,6.3075));
#2814=CARTESIAN_POINT('Ctrl Pts',(4.,-1.65685424949238,6.229375));
#2815=CARTESIAN_POINT('Ctrl Pts',(2.82842712474619,-2.82842712474619,6.15125));
#2816=CARTESIAN_POINT('Ctrl Pts',(1.65685424949238,-4.,6.073125));
#2817=CARTESIAN_POINT('Ctrl Pts',(4.89858719658941E-16,-4.,5.995));
#2818=CARTESIAN_POINT('Ctrl Pts',(-1.65685424949238,-4.,5.916875));
#2819=CARTESIAN_POINT('Ctrl Pts',(-2.82842712474619,-2.82842712474619,5.83875));
#2820=CARTESIAN_POINT('Ctrl Pts',(-4.,-1.65685424949238,5.760625));
#2821=CARTESIAN_POINT('Ctrl Pts',(-4.,-7.34788079488412E-16,5.6825));
#2822=CARTESIAN_POINT('Ctrl Pts',(-4.,1.65685424949238,5.604375));
#2823=CARTESIAN_POINT('Ctrl Pts',(-2.82842712474619,2.82842712474619,5.52625));
#2824=CARTESIAN_POINT('Ctrl Pts',(-1.65685424949238,4.,5.448125));
#2825=CARTESIAN_POINT('Ctrl Pts',(0.,4.,5.37));
#2826=CARTESIAN_POINT('Ctrl Pts',(1.65685424949238,4.,5.291875));
#2827=CARTESIAN_POINT('Ctrl Pts',(2.82842712474619,2.82842712474619,5.21375));
#2828=CARTESIAN_POINT('Ctrl Pts',(4.,1.65685424949238,5.135625));
#2829=CARTESIAN_POINT('Ctrl Pts',(4.,2.44929359829471E-16,5.0575));
#2830=CARTESIAN_POINT('Ctrl Pts',(4.,-1.65685424949238,4.979375));
#2831=CARTESIAN_POINT('Ctrl Pts',(2.82842712474619,-2.82842712474619,4.90125));
#2832=CARTESIAN_POINT('Ctrl Pts',(1.65685424949238,-4.,4.823125));
#2833=CARTESIAN_POINT('Ctrl Pts',(4.89858719658941E-16,-4.,4.745));
#2834=CARTESIAN_POINT('Ctrl Pts',(-1.65685424949238,-4.,4.666875));
#2835=CARTESIAN_POINT('Ctrl Pts',(-2.82842712474619,-2.82842712474619,4.58875));
#2836=CARTESIAN_POINT('Ctrl Pts',(-4.,-1.65685424949238,4.510625));
#2837=CARTESIAN_POINT('Ctrl Pts',(-4.,-7.34788079488412E-16,4.4325));
#2838=CARTESIAN_POINT('Ctrl Pts',(-4.,1.65685424949238,4.354375));
#2839=CARTESIAN_POINT('Ctrl Pts',(-2.82842712474619,2.82842712474619,4.27625));
#2840=CARTESIAN_POINT('Ctrl Pts',(-1.65685424949238,4.,4.198125));
#2841=CARTESIAN_POINT('Ctrl Pts',(0.,4.,4.12));
#2842=CARTESIAN_POINT('Ctrl Pts',(1.65685424949238,4.,4.041875));
#2843=CARTESIAN_POINT('Ctrl Pts',(2.82842712474619,2.82842712474619,3.96375));
#2844=CARTESIAN_POINT('Ctrl Pts',(4.,1.65685424949238,3.885625));
#2845=CARTESIAN_POINT('Ctrl Pts',(4.,2.44929359829471E-16,3.8075));
#2846=CARTESIAN_POINT('Ctrl Pts',(4.,-1.65685424949238,3.729375));
#2847=CARTESIAN_POINT('Ctrl Pts',(2.82842712474619,-2.82842712474619,3.65125));
#2848=CARTESIAN_POINT('Ctrl Pts',(1.65685424949238,-4.,3.573125));
#2849=CARTESIAN_POINT('Ctrl Pts',(4.89858719658941E-16,-4.,3.495));
#2850=CARTESIAN_POINT('Ctrl Pts',(-1.65685424949238,-4.,3.416875));
#2851=CARTESIAN_POINT('Ctrl Pts',(-2.82842712474619,-2.82842712474619,3.33875));
#2852=CARTESIAN_POINT('Ctrl Pts',(-4.,-1.65685424949238,3.260625));
#2853=CARTESIAN_POINT('Ctrl Pts',(-4.,-7.34788079488412E-16,3.1825));
#2854=CARTESIAN_POINT('Ctrl Pts',(-4.,1.65685424949238,3.104375));
#2855=CARTESIAN_POINT('Ctrl Pts',(-2.82842712474619,2.82842712474619,3.02625));
#2856=CARTESIAN_POINT('Ctrl Pts',(-1.65685424949238,4.,2.948125));
#2857=CARTESIAN_POINT('Ctrl Pts',(0.,4.,2.87));
#2858=CARTESIAN_POINT('Ctrl Pts',(1.65685424949238,4.,2.791875));
#2859=CARTESIAN_POINT('Ctrl Pts',(2.82842712474619,2.82842712474619,2.71375));
#2860=CARTESIAN_POINT('Ctrl Pts',(4.,1.65685424949238,2.635625));
#2861=CARTESIAN_POINT('Ctrl Pts',(4.,2.44929359829471E-16,2.5575));
#2862=CARTESIAN_POINT('Ctrl Pts',(4.,-1.65685424949238,2.479375));
#2863=CARTESIAN_POINT('Ctrl Pts',(2.82842712474619,-2.82842712474619,2.40125));
#2864=CARTESIAN_POINT('Ctrl Pts',(1.65685424949238,-4.,2.323125));
#2865=CARTESIAN_POINT('Ctrl Pts',(4.89858719658941E-16,-4.,2.245));
#2866=CARTESIAN_POINT('Ctrl Pts',(-1.65685424949238,-4.,2.166875));
#2867=CARTESIAN_POINT('Ctrl Pts',(-2.82842712474619,-2.82842712474619,2.08875));
#2868=CARTESIAN_POINT('Ctrl Pts',(-4.,-1.65685424949238,2.010625));
#2869=CARTESIAN_POINT('Ctrl Pts',(-4.,-7.34788079488412E-16,1.9325));
#2870=CARTESIAN_POINT('Ctrl Pts',(-4.,1.65685424949238,1.854375));
#2871=CARTESIAN_POINT('Ctrl Pts',(-2.82842712474619,2.82842712474619,1.77625));
#2872=CARTESIAN_POINT('Ctrl Pts',(-1.65685424949238,4.,1.698125));
#2873=CARTESIAN_POINT('Ctrl Pts',(0.,4.,1.62));
#2874=CARTESIAN_POINT('Ctrl Pts',(1.65685424949238,4.,1.541875));
#2875=CARTESIAN_POINT('Ctrl Pts',(2.82842712474619,2.82842712474619,1.46375));
#2876=CARTESIAN_POINT('Ctrl Pts',(4.,1.65685424949238,1.385625));
#2877=CARTESIAN_POINT('Ctrl Pts',(4.,2.44929359829471E-16,1.3075));
#2878=CARTESIAN_POINT('Ctrl Pts',(4.,-1.65685424949238,1.229375));
#2879=CARTESIAN_POINT('Ctrl Pts',(2.82842712474619,-2.82842712474619,1.15125));
#2880=CARTESIAN_POINT('Ctrl Pts',(1.65685424949238,-4.,1.073125));
#2881=CARTESIAN_POINT('Ctrl Pts',(4.89858719658941E-16,-4.,0.995));
#2882=CARTESIAN_POINT('Ctrl Pts',(-1.65685424949238,-4.,0.916875));
#2883=CARTESIAN_POINT('Ctrl Pts',(-2.82842712474619,-2.82842712474619,0.83875));
#2884=CARTESIAN_POINT('Ctrl Pts',(-4.,-1.65685424949238,0.760625));
#2885=CARTESIAN_POINT('Ctrl Pts',(-4.,-7.34788079488412E-16,0.6825));
#2886=CARTESIAN_POINT('Ctrl Pts',(-4.,1.65685424949238,0.604375));
#2887=CARTESIAN_POINT('Ctrl Pts',(-2.82842712474619,2.82842712474619,0.52625));
#2888=CARTESIAN_POINT('Ctrl Pts',(-1.65685424949238,4.,0.448125));
#2889=CARTESIAN_POINT('Ctrl Pts',(0.,4.,0.37));
#2890=CARTESIAN_POINT('Ctrl Pts',(1.65685424949238,4.,0.291875));
#2891=CARTESIAN_POINT('Ctrl Pts',(2.82842712474619,2.82842712474619,0.21375));
#2892=CARTESIAN_POINT('Ctrl Pts',(4.,1.65685424949238,0.135624999999999));
#2893=CARTESIAN_POINT('Ctrl Pts',(4.,2.44929359829471E-16,0.0575000000000003));
#2894=CARTESIAN_POINT('Ctrl Pts',(4.,-1.65685424949238,-0.0206249999999998));
#2895=CARTESIAN_POINT('Ctrl Pts',(2.82842712474619,-2.82842712474619,-0.0987499999999999));
#2896=CARTESIAN_POINT('Ctrl Pts',(1.65685424949238,-4.,-0.176875));
#2897=CARTESIAN_POINT('Ctrl Pts',(4.89858719658941E-16,-4.,-0.255));
#2898=CARTESIAN_POINT('Ctrl Pts',(-1.65685424949238,-4.,-0.333125));
#2899=CARTESIAN_POINT('Ctrl Pts',(-2.82842712474619,-2.82842712474619,-0.41125));
#2900=CARTESIAN_POINT('Ctrl Pts',(-4.,-1.65685424949238,-0.489375));
#2901=CARTESIAN_POINT('Ctrl Pts',(-4.,-7.34788079488412E-16,-0.5675));
#2902=CARTESIAN_POINT('Ctrl Pts',(-4.,1.65685424949238,-0.645625000000001));
#2903=CARTESIAN_POINT('Ctrl Pts',(-2.82842712474619,2.82842712474619,-0.723750000000001));
#2904=CARTESIAN_POINT('Ctrl Pts',(-1.65685424949238,4.,-0.801875000000001));
#2905=CARTESIAN_POINT('Ctrl Pts',(0.,4.,-0.88));
#2906=CARTESIAN_POINT('Ctrl Pts',(-1.92533487773279,-3.50614968428127,5.89456992403025));
#2907=CARTESIAN_POINT('Ctrl Pts',(-2.42519093634574,-3.23166331314664,5.86563934498587));
#2908=CARTESIAN_POINT('Ctrl Pts',(-2.82842712474619,-2.82842712474619,5.83875));
#2909=CARTESIAN_POINT('Ctrl Pts',(-4.,-1.65685424949238,5.760625));
#2910=CARTESIAN_POINT('Ctrl Pts',(-4.,-7.34788079488412E-16,5.6825));
#2911=CARTESIAN_POINT('Ctrl Pts',(-4.,1.65685424949238,5.604375));
#2912=CARTESIAN_POINT('Ctrl Pts',(-2.82842712474619,2.82842712474619,5.52625));
#2913=CARTESIAN_POINT('Ctrl Pts',(-1.65685424949238,4.,5.448125));
#2914=CARTESIAN_POINT('Ctrl Pts',(0.,4.,5.37));
#2915=CARTESIAN_POINT('Ctrl Pts',(1.65685424949238,4.,5.291875));
#2916=CARTESIAN_POINT('Ctrl Pts',(2.82842712474619,2.82842712474619,5.21375));
#2917=CARTESIAN_POINT('Ctrl Pts',(4.,1.65685424949238,5.135625));
#2918=CARTESIAN_POINT('Ctrl Pts',(4.,2.44929359829471E-16,5.0575));
#2919=CARTESIAN_POINT('Ctrl Pts',(4.,-1.65685424949238,4.979375));
#2920=CARTESIAN_POINT('Ctrl Pts',(2.82842712474619,-2.82842712474619,4.90125));
#2921=CARTESIAN_POINT('Ctrl Pts',(1.65685424949238,-4.,4.823125));
#2922=CARTESIAN_POINT('Ctrl Pts',(4.89858719658941E-16,-4.,4.745));
#2923=CARTESIAN_POINT('Ctrl Pts',(-1.65685424949238,-4.,4.666875));
#2924=CARTESIAN_POINT('Ctrl Pts',(-2.82842712474619,-2.82842712474619,4.58875));
#2925=CARTESIAN_POINT('Ctrl Pts',(-4.,-1.65685424949238,4.510625));
#2926=CARTESIAN_POINT('Ctrl Pts',(-4.,-7.34788079488412E-16,4.4325));
#2927=CARTESIAN_POINT('Ctrl Pts',(-4.,1.65685424949238,4.354375));
#2928=CARTESIAN_POINT('Ctrl Pts',(-2.82842712474619,2.82842712474619,4.27625));
#2929=CARTESIAN_POINT('Ctrl Pts',(-1.65685424949238,4.,4.198125));
#2930=CARTESIAN_POINT('Ctrl Pts',(0.,4.,4.12));
#2931=CARTESIAN_POINT('Ctrl Pts',(1.65685424949238,4.,4.041875));
#2932=CARTESIAN_POINT('Ctrl Pts',(2.82842712474619,2.82842712474619,3.96375));
#2933=CARTESIAN_POINT('Ctrl Pts',(4.,1.65685424949238,3.885625));
#2934=CARTESIAN_POINT('Ctrl Pts',(4.,2.44929359829471E-16,3.8075));
#2935=CARTESIAN_POINT('Ctrl Pts',(4.,-1.65685424949238,3.729375));
#2936=CARTESIAN_POINT('Ctrl Pts',(2.82842712474619,-2.82842712474619,3.65125));
#2937=CARTESIAN_POINT('Ctrl Pts',(1.65685424949238,-4.,3.573125));
#2938=CARTESIAN_POINT('Ctrl Pts',(4.89858719658941E-16,-4.,3.495));
#2939=CARTESIAN_POINT('Ctrl Pts',(-1.65685424949238,-4.,3.416875));
#2940=CARTESIAN_POINT('Ctrl Pts',(-2.82842712474619,-2.82842712474619,3.33875));
#2941=CARTESIAN_POINT('Ctrl Pts',(-4.,-1.65685424949238,3.260625));
#2942=CARTESIAN_POINT('Ctrl Pts',(-4.,-7.34788079488412E-16,3.1825));
#2943=CARTESIAN_POINT('Ctrl Pts',(-4.,1.65685424949238,3.104375));
#2944=CARTESIAN_POINT('Ctrl Pts',(-2.82842712474619,2.82842712474619,3.02625));
#2945=CARTESIAN_POINT('Ctrl Pts',(-1.65685424949238,4.,2.948125));
#2946=CARTESIAN_POINT('Ctrl Pts',(0.,4.,2.87));
#2947=CARTESIAN_POINT('Ctrl Pts',(1.65685424949238,4.,2.791875));
#2948=CARTESIAN_POINT('Ctrl Pts',(2.82842712474619,2.82842712474619,2.71375));
#2949=CARTESIAN_POINT('Ctrl Pts',(4.,1.65685424949238,2.635625));
#2950=CARTESIAN_POINT('Ctrl Pts',(4.,2.44929359829471E-16,2.5575));
#2951=CARTESIAN_POINT('Ctrl Pts',(4.,-1.65685424949238,2.479375));
#2952=CARTESIAN_POINT('Ctrl Pts',(2.82842712474619,-2.82842712474619,2.40125));
#2953=CARTESIAN_POINT('Ctrl Pts',(1.65685424949238,-4.,2.323125));
#2954=CARTESIAN_POINT('Ctrl Pts',(4.89858719658941E-16,-4.,2.245));
#2955=CARTESIAN_POINT('Ctrl Pts',(-1.65685424949238,-4.,2.166875));
#2956=CARTESIAN_POINT('Ctrl Pts',(-2.82842712474619,-2.82842712474619,2.08875));
#2957=CARTESIAN_POINT('Ctrl Pts',(-4.,-1.65685424949238,2.010625));
#2958=CARTESIAN_POINT('Ctrl Pts',(-4.,-7.34788079488412E-16,1.9325));
#2959=CARTESIAN_POINT('Ctrl Pts',(-4.,1.65685424949238,1.854375));
#2960=CARTESIAN_POINT('Ctrl Pts',(-2.82842712474619,2.82842712474619,1.77625));
#2961=CARTESIAN_POINT('Ctrl Pts',(-1.65685424949238,4.,1.698125));
#2962=CARTESIAN_POINT('Ctrl Pts',(0.,4.,1.62));
#2963=CARTESIAN_POINT('Ctrl Pts',(1.65685424949238,4.,1.541875));
#2964=CARTESIAN_POINT('Ctrl Pts',(2.82842712474619,2.82842712474619,1.46375));
#2965=CARTESIAN_POINT('Ctrl Pts',(4.,1.65685424949238,1.385625));
#2966=CARTESIAN_POINT('Ctrl Pts',(4.,2.44929359829471E-16,1.3075));
#2967=CARTESIAN_POINT('Ctrl Pts',(4.,-1.65685424949238,1.229375));
#2968=CARTESIAN_POINT('Ctrl Pts',(2.82842712474619,-2.82842712474619,1.15125));
#2969=CARTESIAN_POINT('Ctrl Pts',(1.65685424949238,-4.,1.073125));
#2970=CARTESIAN_POINT('Ctrl Pts',(4.89858719658941E-16,-4.,0.995));
#2971=CARTESIAN_POINT('Ctrl Pts',(-1.65685424949238,-4.,0.916875));
#2972=CARTESIAN_POINT('Ctrl Pts',(-2.82842712474619,-2.82842712474619,0.83875));
#2973=CARTESIAN_POINT('Ctrl Pts',(-4.,-1.65685424949238,0.760625));
#2974=CARTESIAN_POINT('Ctrl Pts',(-4.,-7.34788079488412E-16,0.6825));
#2975=CARTESIAN_POINT('Ctrl Pts',(-4.,1.65685424949238,0.604375));
#2976=CARTESIAN_POINT('Ctrl Pts',(-2.82842712474619,2.82842712474619,0.52625));
#2977=CARTESIAN_POINT('Ctrl Pts',(-1.65685424949238,4.,0.448125));
#2978=CARTESIAN_POINT('Ctrl Pts',(0.,4.,0.37));
#2979=CARTESIAN_POINT('Ctrl Pts',(1.65685424949238,4.,0.291875));
#2980=CARTESIAN_POINT('Ctrl Pts',(2.82842712474619,2.82842712474619,0.21375));
#2981=CARTESIAN_POINT('Ctrl Pts',(3.6129669626084,2.04388728688398,0.161433856354469));
#2982=CARTESIAN_POINT('Ctrl Pts',(3.88127665353657,0.967311500351366,0.105430075969749));
#2983=CARTESIAN_POINT('Ctrl Pts',(0.,4.,6.62));
#2984=CARTESIAN_POINT('Ctrl Pts',(1.65685424949238,4.,6.541875));
#2985=CARTESIAN_POINT('Ctrl Pts',(2.82842712474619,2.82842712474619,6.46375));
#2986=CARTESIAN_POINT('Ctrl Pts',(4.,1.65685424949238,6.385625));
#2987=CARTESIAN_POINT('Ctrl Pts',(4.,2.44929359829471E-16,6.3075));
#2988=CARTESIAN_POINT('Ctrl Pts',(4.,-1.65685424949238,6.229375));
#2989=CARTESIAN_POINT('Ctrl Pts',(2.82842712474619,-2.82842712474619,6.15125));
#2990=CARTESIAN_POINT('Ctrl Pts',(1.65685424949238,-4.,6.073125));
#2991=CARTESIAN_POINT('Ctrl Pts',(4.89858719658941E-16,-4.,5.995));
#2992=CARTESIAN_POINT('Ctrl Pts',(-1.65685424949238,-4.,5.916875));
#2993=CARTESIAN_POINT('Ctrl Pts',(-2.82842712474619,-2.82842712474619,5.83875));
#2994=CARTESIAN_POINT('Ctrl Pts',(-4.,-1.65685424949238,5.760625));
#2995=CARTESIAN_POINT('Ctrl Pts',(-4.,-7.34788079488412E-16,5.6825));
#2996=CARTESIAN_POINT('Ctrl Pts',(-4.,1.65685424949238,5.604375));
#2997=CARTESIAN_POINT('Ctrl Pts',(-2.82842712474619,2.82842712474619,5.52625));
#2998=CARTESIAN_POINT('Ctrl Pts',(-1.65685424949238,4.,5.448125));
#2999=CARTESIAN_POINT('Ctrl Pts',(0.,4.,5.37));
#3000=CARTESIAN_POINT('Ctrl Pts',(1.65685424949238,4.,5.291875));
#3001=CARTESIAN_POINT('Ctrl Pts',(2.82842712474619,2.82842712474619,5.21375));
#3002=CARTESIAN_POINT('Ctrl Pts',(4.,1.65685424949238,5.135625));
#3003=CARTESIAN_POINT('Ctrl Pts',(4.,2.44929359829471E-16,5.0575));
#3004=CARTESIAN_POINT('Ctrl Pts',(4.,-1.65685424949238,4.979375));
#3005=CARTESIAN_POINT('Ctrl Pts',(2.82842712474619,-2.82842712474619,4.90125));
#3006=CARTESIAN_POINT('Ctrl Pts',(1.65685424949238,-4.,4.823125));
#3007=CARTESIAN_POINT('Ctrl Pts',(4.89858719658941E-16,-4.,4.745));
#3008=CARTESIAN_POINT('Ctrl Pts',(-1.65685424949238,-4.,4.666875));
#3009=CARTESIAN_POINT('Ctrl Pts',(-2.82842712474619,-2.82842712474619,4.58875));
#3010=CARTESIAN_POINT('Ctrl Pts',(-4.,-1.65685424949238,4.510625));
#3011=CARTESIAN_POINT('Ctrl Pts',(-4.,-7.34788079488412E-16,4.4325));
#3012=CARTESIAN_POINT('Ctrl Pts',(-4.,1.65685424949238,4.354375));
#3013=CARTESIAN_POINT('Ctrl Pts',(-2.82842712474619,2.82842712474619,4.27625));
#3014=CARTESIAN_POINT('Ctrl Pts',(-1.65685424949238,4.,4.198125));
#3015=CARTESIAN_POINT('Ctrl Pts',(0.,4.,4.12));
#3016=CARTESIAN_POINT('Ctrl Pts',(1.65685424949238,4.,4.041875));
#3017=CARTESIAN_POINT('Ctrl Pts',(2.82842712474619,2.82842712474619,3.96375));
#3018=CARTESIAN_POINT('Ctrl Pts',(4.,1.65685424949238,3.885625));
#3019=CARTESIAN_POINT('Ctrl Pts',(4.,2.44929359829471E-16,3.8075));
#3020=CARTESIAN_POINT('Ctrl Pts',(4.,-1.65685424949238,3.729375));
#3021=CARTESIAN_POINT('Ctrl Pts',(2.82842712474619,-2.82842712474619,3.65125));
#3022=CARTESIAN_POINT('Ctrl Pts',(1.65685424949238,-4.,3.573125));
#3023=CARTESIAN_POINT('Ctrl Pts',(4.89858719658941E-16,-4.,3.495));
#3024=CARTESIAN_POINT('Ctrl Pts',(-1.65685424949238,-4.,3.416875));
#3025=CARTESIAN_POINT('Ctrl Pts',(-2.82842712474619,-2.82842712474619,3.33875));
#3026=CARTESIAN_POINT('Ctrl Pts',(-4.,-1.65685424949238,3.260625));
#3027=CARTESIAN_POINT('Ctrl Pts',(-4.,-7.34788079488412E-16,3.1825));
#3028=CARTESIAN_POINT('Ctrl Pts',(-4.,1.65685424949238,3.104375));
#3029=CARTESIAN_POINT('Ctrl Pts',(-2.82842712474619,2.82842712474619,3.02625));
#3030=CARTESIAN_POINT('Ctrl Pts',(-1.65685424949238,4.,2.948125));
#3031=CARTESIAN_POINT('Ctrl Pts',(0.,4.,2.87));
#3032=CARTESIAN_POINT('Ctrl Pts',(1.65685424949238,4.,2.791875));
#3033=CARTESIAN_POINT('Ctrl Pts',(2.82842712474619,2.82842712474619,2.71375));
#3034=CARTESIAN_POINT('Ctrl Pts',(4.,1.65685424949238,2.635625));
#3035=CARTESIAN_POINT('Ctrl Pts',(4.,2.44929359829471E-16,2.5575));
#3036=CARTESIAN_POINT('Ctrl Pts',(4.,-1.65685424949238,2.479375));
#3037=CARTESIAN_POINT('Ctrl Pts',(2.82842712474619,-2.82842712474619,2.40125));
#3038=CARTESIAN_POINT('Ctrl Pts',(1.65685424949238,-4.,2.323125));
#3039=CARTESIAN_POINT('Ctrl Pts',(4.89858719658941E-16,-4.,2.245));
#3040=CARTESIAN_POINT('Ctrl Pts',(-1.65685424949238,-4.,2.166875));
#3041=CARTESIAN_POINT('Ctrl Pts',(-2.82842712474619,-2.82842712474619,2.08875));
#3042=CARTESIAN_POINT('Ctrl Pts',(-4.,-1.65685424949238,2.010625));
#3043=CARTESIAN_POINT('Ctrl Pts',(-4.,-7.34788079488412E-16,1.9325));
#3044=CARTESIAN_POINT('Ctrl Pts',(-4.,1.65685424949238,1.854375));
#3045=CARTESIAN_POINT('Ctrl Pts',(-2.82842712474619,2.82842712474619,1.77625));
#3046=CARTESIAN_POINT('Ctrl Pts',(-1.65685424949238,4.,1.698125));
#3047=CARTESIAN_POINT('Ctrl Pts',(0.,4.,1.62));
#3048=CARTESIAN_POINT('Ctrl Pts',(1.65685424949238,4.,1.541875));
#3049=CARTESIAN_POINT('Ctrl Pts',(2.82842712474619,2.82842712474619,1.46375));
#3050=CARTESIAN_POINT('Ctrl Pts',(4.,1.65685424949238,1.385625));
#3051=CARTESIAN_POINT('Ctrl Pts',(4.,2.44929359829471E-16,1.3075));
#3052=CARTESIAN_POINT('Ctrl Pts',(4.,-1.65685424949238,1.229375));
#3053=CARTESIAN_POINT('Ctrl Pts',(2.82842712474619,-2.82842712474619,1.15125));
#3054=CARTESIAN_POINT('Ctrl Pts',(1.65685424949238,-4.,1.073125));
#3055=CARTESIAN_POINT('Ctrl Pts',(4.89858719658941E-16,-4.,0.995));
#3056=CARTESIAN_POINT('Ctrl Pts',(-1.65685424949238,-4.,0.916875));
#3057=CARTESIAN_POINT('Ctrl Pts',(-2.82842712474619,-2.82842712474619,0.83875));
#3058=CARTESIAN_POINT('Ctrl Pts',(-4.,-1.65685424949238,0.760625));
#3059=CARTESIAN_POINT('Ctrl Pts',(-4.,-7.34788079488412E-16,0.6825));
#3060=CARTESIAN_POINT('Ctrl Pts',(-4.,1.65685424949238,0.604375));
#3061=CARTESIAN_POINT('Ctrl Pts',(-2.82842712474619,2.82842712474619,0.52625));
#3062=CARTESIAN_POINT('Ctrl Pts',(-1.65685424949238,4.,0.448125));
#3063=CARTESIAN_POINT('Ctrl Pts',(0.,4.,0.37));
#3064=CARTESIAN_POINT('Ctrl Pts',(1.65685424949238,4.,0.291875));
#3065=CARTESIAN_POINT('Ctrl Pts',(2.82842712474619,2.82842712474619,0.21375));
#3066=CARTESIAN_POINT('Ctrl Pts',(4.,1.65685424949238,0.135624999999999));
#3067=CARTESIAN_POINT('Ctrl Pts',(4.,2.44929359829471E-16,0.0575000000000003));
#3068=CARTESIAN_POINT('Ctrl Pts',(4.,-1.65685424949238,-0.0206249999999998));
#3069=CARTESIAN_POINT('Ctrl Pts',(2.82842712474619,-2.82842712474619,-0.0987499999999999));
#3070=CARTESIAN_POINT('Ctrl Pts',(1.65685424949238,-4.,-0.176875));
#3071=CARTESIAN_POINT('Ctrl Pts',(4.89858719658941E-16,-4.,-0.255));
#3072=CARTESIAN_POINT('Ctrl Pts',(-1.65685424949238,-4.,-0.333125));
#3073=CARTESIAN_POINT('Ctrl Pts',(-2.82842712474619,-2.82842712474619,-0.41125));
#3074=CARTESIAN_POINT('Ctrl Pts',(-4.,-1.65685424949238,-0.489375));
#3075=CARTESIAN_POINT('Ctrl Pts',(-4.,-7.34788079488412E-16,-0.5675));
#3076=CARTESIAN_POINT('Ctrl Pts',(-4.,1.65685424949238,-0.645625000000001));
#3077=CARTESIAN_POINT('Ctrl Pts',(-2.82842712474619,2.82842712474619,-0.723750000000001));
#3078=CARTESIAN_POINT('Ctrl Pts',(-1.65685424949238,4.,-0.801875000000001));
#3079=CARTESIAN_POINT('Ctrl Pts',(0.,4.,-0.88));
#3080=CARTESIAN_POINT('Ctrl Pts',(0.,3.39995998131687,7.24004135263924));
#3081=CARTESIAN_POINT('Ctrl Pts',(1.40830953578722,3.39995998131687,7.16191635263924));
#3082=CARTESIAN_POINT('Ctrl Pts',(2.40413475855205,2.40413475855205,7.08379135263924));
#3083=CARTESIAN_POINT('Ctrl Pts',(3.39995998131687,1.40830953578722,7.00566635263924));
#3084=CARTESIAN_POINT('Ctrl Pts',(3.39995998131687,2.0818750541744E-16,
6.92754135263924));
#3085=CARTESIAN_POINT('Ctrl Pts',(3.39995998131687,-1.40830953578722,6.84941635263924));
#3086=CARTESIAN_POINT('Ctrl Pts',(2.40413475855205,-2.40413475855205,6.77129135263923));
#3087=CARTESIAN_POINT('Ctrl Pts',(1.40830953578722,-3.39995998131687,6.69316635263924));
#3088=CARTESIAN_POINT('Ctrl Pts',(4.1637501083488E-16,-3.39995998131687,
6.61504135263924));
#3089=CARTESIAN_POINT('Ctrl Pts',(-1.40830953578722,-3.39995998131687,6.53691635263924));
#3090=CARTESIAN_POINT('Ctrl Pts',(-2.40413475855205,-2.40413475855205,6.45879135263924));
#3091=CARTESIAN_POINT('Ctrl Pts',(-3.39995998131687,-1.40830953578722,6.38066635263924));
#3092=CARTESIAN_POINT('Ctrl Pts',(-3.39995998131687,-6.2456251625232E-16,
6.30254135263924));
#3093=CARTESIAN_POINT('Ctrl Pts',(-3.39995998131687,1.40830953578722,6.22441635263923));
#3094=CARTESIAN_POINT('Ctrl Pts',(-2.40413475855205,2.40413475855204,6.14629135263924));
#3095=CARTESIAN_POINT('Ctrl Pts',(-1.40830953578722,3.39995998131687,6.06816635263924));
#3096=CARTESIAN_POINT('Ctrl Pts',(0.,3.39995998131687,5.99004135263923));
#3097=CARTESIAN_POINT('Ctrl Pts',(1.40830953578722,3.39995998131687,5.91191635263923));
#3098=CARTESIAN_POINT('Ctrl Pts',(2.40413475855205,2.40413475855205,5.83379135263924));
#3099=CARTESIAN_POINT('Ctrl Pts',(3.39995998131687,1.40830953578722,5.75566635263924));
#3100=CARTESIAN_POINT('Ctrl Pts',(3.39995998131687,2.0818750541744E-16,
5.67754135263924));
#3101=CARTESIAN_POINT('Ctrl Pts',(3.39995998131687,-1.40830953578722,5.59941635263924));
#3102=CARTESIAN_POINT('Ctrl Pts',(2.40413475855205,-2.40413475855205,5.52129135263924));
#3103=CARTESIAN_POINT('Ctrl Pts',(1.40830953578722,-3.39995998131687,5.44316635263924));
#3104=CARTESIAN_POINT('Ctrl Pts',(4.1637501083488E-16,-3.39995998131687,
5.36504135263924));
#3105=CARTESIAN_POINT('Ctrl Pts',(-1.40830953578722,-3.39995998131687,5.28691635263924));
#3106=CARTESIAN_POINT('Ctrl Pts',(-2.40413475855205,-2.40413475855205,5.20879135263924));
#3107=CARTESIAN_POINT('Ctrl Pts',(-3.39995998131687,-1.40830953578722,5.13066635263924));
#3108=CARTESIAN_POINT('Ctrl Pts',(-3.39995998131687,-6.2456251625232E-16,
5.05254135263924));
#3109=CARTESIAN_POINT('Ctrl Pts',(-3.39995998131687,1.40830953578722,4.97441635263923));
#3110=CARTESIAN_POINT('Ctrl Pts',(-2.40413475855205,2.40413475855204,4.89629135263924));
#3111=CARTESIAN_POINT('Ctrl Pts',(-1.40830953578722,3.39995998131687,4.81816635263924));
#3112=CARTESIAN_POINT('Ctrl Pts',(0.,3.39995998131687,4.74004135263923));
#3113=CARTESIAN_POINT('Ctrl Pts',(1.40830953578722,3.39995998131687,4.66191635263923));
#3114=CARTESIAN_POINT('Ctrl Pts',(2.40413475855205,2.40413475855205,4.58379135263924));
#3115=CARTESIAN_POINT('Ctrl Pts',(3.39995998131687,1.40830953578722,4.50566635263923));
#3116=CARTESIAN_POINT('Ctrl Pts',(3.39995998131687,2.0818750541744E-16,
4.42754135263924));
#3117=CARTESIAN_POINT('Ctrl Pts',(3.39995998131687,-1.40830953578722,4.34941635263924));
#3118=CARTESIAN_POINT('Ctrl Pts',(2.40413475855205,-2.40413475855205,4.27129135263924));
#3119=CARTESIAN_POINT('Ctrl Pts',(1.40830953578722,-3.39995998131687,4.19316635263924));
#3120=CARTESIAN_POINT('Ctrl Pts',(4.1637501083488E-16,-3.39995998131687,
4.11504135263923));
#3121=CARTESIAN_POINT('Ctrl Pts',(-1.40830953578722,-3.39995998131687,4.03691635263924));
#3122=CARTESIAN_POINT('Ctrl Pts',(-2.40413475855205,-2.40413475855205,3.95879135263924));
#3123=CARTESIAN_POINT('Ctrl Pts',(-3.39995998131687,-1.40830953578722,3.88066635263924));
#3124=CARTESIAN_POINT('Ctrl Pts',(-3.39995998131687,-6.2456251625232E-16,
3.80254135263923));
#3125=CARTESIAN_POINT('Ctrl Pts',(-3.39995998131687,1.40830953578722,3.72441635263924));
#3126=CARTESIAN_POINT('Ctrl Pts',(-2.40413475855205,2.40413475855204,3.64629135263924));
#3127=CARTESIAN_POINT('Ctrl Pts',(-1.40830953578722,3.39995998131687,3.56816635263924));
#3128=CARTESIAN_POINT('Ctrl Pts',(0.,3.39995998131687,3.49004135263924));
#3129=CARTESIAN_POINT('Ctrl Pts',(1.40830953578722,3.39995998131687,3.41191635263924));
#3130=CARTESIAN_POINT('Ctrl Pts',(2.40413475855205,2.40413475855205,3.33379135263924));
#3131=CARTESIAN_POINT('Ctrl Pts',(3.39995998131687,1.40830953578722,3.25566635263924));
#3132=CARTESIAN_POINT('Ctrl Pts',(3.39995998131687,2.0818750541744E-16,
3.17754135263923));
#3133=CARTESIAN_POINT('Ctrl Pts',(3.39995998131687,-1.40830953578722,3.09941635263924));
#3134=CARTESIAN_POINT('Ctrl Pts',(2.40413475855205,-2.40413475855205,3.02129135263924));
#3135=CARTESIAN_POINT('Ctrl Pts',(1.40830953578722,-3.39995998131687,2.94316635263924));
#3136=CARTESIAN_POINT('Ctrl Pts',(4.1637501083488E-16,-3.39995998131687,
2.86504135263923));
#3137=CARTESIAN_POINT('Ctrl Pts',(-1.40830953578722,-3.39995998131687,2.78691635263924));
#3138=CARTESIAN_POINT('Ctrl Pts',(-2.40413475855205,-2.40413475855205,2.70879135263924));
#3139=CARTESIAN_POINT('Ctrl Pts',(-3.39995998131687,-1.40830953578722,2.63066635263924));
#3140=CARTESIAN_POINT('Ctrl Pts',(-3.39995998131687,-6.2456251625232E-16,
2.55254135263924));
#3141=CARTESIAN_POINT('Ctrl Pts',(-3.39995998131687,1.40830953578722,2.47441635263924));
#3142=CARTESIAN_POINT('Ctrl Pts',(-2.40413475855205,2.40413475855204,2.39629135263924));
#3143=CARTESIAN_POINT('Ctrl Pts',(-1.40830953578722,3.39995998131687,2.31816635263924));
#3144=CARTESIAN_POINT('Ctrl Pts',(0.,3.39995998131687,2.24004135263924));
#3145=CARTESIAN_POINT('Ctrl Pts',(1.40830953578722,3.39995998131687,2.16191635263924));
#3146=CARTESIAN_POINT('Ctrl Pts',(2.40413475855205,2.40413475855205,2.08379135263924));
#3147=CARTESIAN_POINT('Ctrl Pts',(3.39995998131687,1.40830953578722,2.00566635263924));
#3148=CARTESIAN_POINT('Ctrl Pts',(3.39995998131687,2.0818750541744E-16,
1.92754135263924));
#3149=CARTESIAN_POINT('Ctrl Pts',(3.39995998131687,-1.40830953578722,1.84941635263924));
#3150=CARTESIAN_POINT('Ctrl Pts',(2.40413475855205,-2.40413475855205,1.77129135263924));
#3151=CARTESIAN_POINT('Ctrl Pts',(1.40830953578722,-3.39995998131687,1.69316635263924));
#3152=CARTESIAN_POINT('Ctrl Pts',(4.1637501083488E-16,-3.39995998131687,
1.61504135263924));
#3153=CARTESIAN_POINT('Ctrl Pts',(-1.40830953578722,-3.39995998131687,1.53691635263924));
#3154=CARTESIAN_POINT('Ctrl Pts',(-2.40413475855205,-2.40413475855205,1.45879135263924));
#3155=CARTESIAN_POINT('Ctrl Pts',(-3.39995998131687,-1.40830953578722,1.38066635263924));
#3156=CARTESIAN_POINT('Ctrl Pts',(-3.39995998131687,-6.2456251625232E-16,
1.30254135263924));
#3157=CARTESIAN_POINT('Ctrl Pts',(-3.39995998131687,1.40830953578722,1.22441635263924));
#3158=CARTESIAN_POINT('Ctrl Pts',(-2.40413475855205,2.40413475855204,1.14629135263924));
#3159=CARTESIAN_POINT('Ctrl Pts',(-1.40830953578722,3.39995998131687,1.06816635263924));
#3160=CARTESIAN_POINT('Ctrl Pts',(0.,3.39995998131687,0.990041352639235));
#3161=CARTESIAN_POINT('Ctrl Pts',(1.40830953578722,3.39995998131687,0.911916352639235));
#3162=CARTESIAN_POINT('Ctrl Pts',(2.40413475855205,2.40413475855205,0.833791352639235));
#3163=CARTESIAN_POINT('Ctrl Pts',(3.39995998131687,1.40830953578722,0.755666352639235));
#3164=CARTESIAN_POINT('Ctrl Pts',(3.39995998131687,2.0818750541744E-16,
0.677541352639236));
#3165=CARTESIAN_POINT('Ctrl Pts',(3.39995998131687,-1.40830953578722,0.599416352639236));
#3166=CARTESIAN_POINT('Ctrl Pts',(2.40413475855205,-2.40413475855205,0.521291352639235));
#3167=CARTESIAN_POINT('Ctrl Pts',(1.40830953578722,-3.39995998131687,0.443166352639235));
#3168=CARTESIAN_POINT('Ctrl Pts',(4.1637501083488E-16,-3.39995998131687,
0.365041352639235));
#3169=CARTESIAN_POINT('Ctrl Pts',(-1.40830953578722,-3.39995998131687,0.286916352639235));
#3170=CARTESIAN_POINT('Ctrl Pts',(-2.40413475855205,-2.40413475855205,0.208791352639235));
#3171=CARTESIAN_POINT('Ctrl Pts',(-3.39995998131687,-1.40830953578722,0.130666352639235));
#3172=CARTESIAN_POINT('Ctrl Pts',(-3.39995998131687,-6.2456251625232E-16,
0.052541352639235));
#3173=CARTESIAN_POINT('Ctrl Pts',(-3.39995998131687,1.40830953578722,-0.0255836473607651));
#3174=CARTESIAN_POINT('Ctrl Pts',(-2.40413475855205,2.40413475855204,-0.103708647360765));
#3175=CARTESIAN_POINT('Ctrl Pts',(-1.40830953578722,3.39995998131687,-0.181833647360765));
#3176=CARTESIAN_POINT('Ctrl Pts',(0.,3.39995998131687,-0.259958647360764));
#3177=CARTESIAN_POINT('',(13.1235599055582,-4.62186957167346,89.));
#3178=CARTESIAN_POINT('',(-6.87644009443938,-4.62186957167707,47.));
#3179=CARTESIAN_POINT('',(-5.34096740217134,-19.0403411831728,53.9999999999967));
#3180=CARTESIAN_POINT('',(-28.8541015546292,-6.96234235151143,9.01661848230447));
#3181=CARTESIAN_POINT('',(-28.8541015546294,-6.96234235151146,9.01661848230385));
#3182=CARTESIAN_POINT('',(21.195247036447,-22.2483349719452,11.0632897219336));
#3183=CARTESIAN_POINT('',(18.8325977313746,-1.88402560390333,11.0634233626401));
#3184=CARTESIAN_POINT('',(-7.88243944455597,4.82471527722763,53.9999999999992));
#3185=CARTESIAN_POINT('',(18.8325977313747,-1.88402560390332,11.0634233626399));
#3186=CARTESIAN_POINT('',(-27.1579054954168,-21.3637020478753,9.12189419440526));
#3187=CARTESIAN_POINT('',(-30.8332681426449,13.4428013419273,9.00938367257674));
#3188=CARTESIAN_POINT('',(17.4887253198488,12.5548501812617,11.0544347041818));
#3189=CARTESIAN_POINT('',(-6.8764400944418,-4.62186957167346,41.));
#3190=CARTESIAN_POINT('',(-8.86543347972561,15.7822317019539,54.0613540751981));
#3191=CARTESIAN_POINT('',(-5.64664943772434,-19.072894315764,53.4847342562298));
#3192=UNCERTAINTY_MEASURE_WITH_UNIT(LENGTH_MEASURE(0.01),#3208,
'DISTANCE_ACCURACY_VALUE',
'Maximum model space distance between geometric entities at asserted c
onnectivities');
#3193=UNCERTAINTY_MEASURE_WITH_UNIT(LENGTH_MEASURE(0.01),#3208,
'DISTANCE_ACCURACY_VALUE',
'Maximum model space distance between geometric entities at asserted c
onnectivities');
#3194=UNCERTAINTY_MEASURE_WITH_UNIT(LENGTH_MEASURE(0.01),#3208,
'DISTANCE_ACCURACY_VALUE',
'Maximum model space distance between geometric entities at asserted c
onnectivities');
#3195=UNCERTAINTY_MEASURE_WITH_UNIT(LENGTH_MEASURE(0.01),#3208,
'DISTANCE_ACCURACY_VALUE',
'Maximum model space distance between geometric entities at asserted c
onnectivities');
#3196=UNCERTAINTY_MEASURE_WITH_UNIT(LENGTH_MEASURE(0.01),#3208,
'DISTANCE_ACCURACY_VALUE',
'Maximum model space distance between geometric entities at asserted c
onnectivities');
#3197=UNCERTAINTY_MEASURE_WITH_UNIT(LENGTH_MEASURE(0.01),#3208,
'DISTANCE_ACCURACY_VALUE',
'Maximum model space distance between geometric entities at asserted c
onnectivities');
#3198=UNCERTAINTY_MEASURE_WITH_UNIT(LENGTH_MEASURE(0.01),#3208,
'DISTANCE_ACCURACY_VALUE',
'Maximum model space distance between geometric entities at asserted c
onnectivities');
#3199=UNCERTAINTY_MEASURE_WITH_UNIT(LENGTH_MEASURE(0.01),#3208,
'DISTANCE_ACCURACY_VALUE',
'Maximum model space distance between geometric entities at asserted c
onnectivities');
#3200=(
GEOMETRIC_REPRESENTATION_CONTEXT(3)
GLOBAL_UNCERTAINTY_ASSIGNED_CONTEXT((#3192))
GLOBAL_UNIT_ASSIGNED_CONTEXT((#3208,#3210,#3211))
REPRESENTATION_CONTEXT('','3D')
);
#3201=(
GEOMETRIC_REPRESENTATION_CONTEXT(3)
GLOBAL_UNCERTAINTY_ASSIGNED_CONTEXT((#3193))
GLOBAL_UNIT_ASSIGNED_CONTEXT((#3208,#3210,#3211))
REPRESENTATION_CONTEXT('','3D')
);
#3202=(
GEOMETRIC_REPRESENTATION_CONTEXT(3)
GLOBAL_UNCERTAINTY_ASSIGNED_CONTEXT((#3194))
GLOBAL_UNIT_ASSIGNED_CONTEXT((#3208,#3210,#3211))
REPRESENTATION_CONTEXT('','3D')
);
#3203=(
GEOMETRIC_REPRESENTATION_CONTEXT(3)
GLOBAL_UNCERTAINTY_ASSIGNED_CONTEXT((#3195))
GLOBAL_UNIT_ASSIGNED_CONTEXT((#3208,#3210,#3211))
REPRESENTATION_CONTEXT('','3D')
);
#3204=(
GEOMETRIC_REPRESENTATION_CONTEXT(3)
GLOBAL_UNCERTAINTY_ASSIGNED_CONTEXT((#3196))
GLOBAL_UNIT_ASSIGNED_CONTEXT((#3208,#3210,#3211))
REPRESENTATION_CONTEXT('','3D')
);
#3205=(
GEOMETRIC_REPRESENTATION_CONTEXT(3)
GLOBAL_UNCERTAINTY_ASSIGNED_CONTEXT((#3197))
GLOBAL_UNIT_ASSIGNED_CONTEXT((#3208,#3210,#3211))
REPRESENTATION_CONTEXT('','3D')
);
#3206=(
GEOMETRIC_REPRESENTATION_CONTEXT(3)
GLOBAL_UNCERTAINTY_ASSIGNED_CONTEXT((#3198))
GLOBAL_UNIT_ASSIGNED_CONTEXT((#3208,#3210,#3211))
REPRESENTATION_CONTEXT('','3D')
);
#3207=(
GEOMETRIC_REPRESENTATION_CONTEXT(3)
GLOBAL_UNCERTAINTY_ASSIGNED_CONTEXT((#3199))
GLOBAL_UNIT_ASSIGNED_CONTEXT((#3208,#3210,#3211))
REPRESENTATION_CONTEXT('','3D')
);
#3208=(
LENGTH_UNIT()
NAMED_UNIT(*)
SI_UNIT(.MILLI.,.METRE.)
);
#3209=(
LENGTH_UNIT()
NAMED_UNIT(*)
SI_UNIT($,.METRE.)
);
#3210=(
NAMED_UNIT(*)
PLANE_ANGLE_UNIT()
SI_UNIT($,.RADIAN.)
);
#3211=(
NAMED_UNIT(*)
SI_UNIT($,.STERADIAN.)
SOLID_ANGLE_UNIT()
);
#3212=SHAPE_DEFINITION_REPRESENTATION(#3219,#3241);
#3213=SHAPE_DEFINITION_REPRESENTATION(#3220,#3242);
#3214=SHAPE_DEFINITION_REPRESENTATION(#3221,#3243);
#3215=SHAPE_DEFINITION_REPRESENTATION(#3222,#3244);
#3216=SHAPE_DEFINITION_REPRESENTATION(#3223,#3245);
#3217=SHAPE_DEFINITION_REPRESENTATION(#3224,#3246);
#3218=SHAPE_DEFINITION_REPRESENTATION(#3225,#3247);
#3219=PRODUCT_DEFINITION_SHAPE('',$,#3249);
#3220=PRODUCT_DEFINITION_SHAPE('',$,#3250);
#3221=PRODUCT_DEFINITION_SHAPE('',$,#3251);
#3222=PRODUCT_DEFINITION_SHAPE('',$,#3252);
#3223=PRODUCT_DEFINITION_SHAPE('',$,#3253);
#3224=PRODUCT_DEFINITION_SHAPE('',$,#3254);
#3225=PRODUCT_DEFINITION_SHAPE('',$,#3255);
#3226=PRODUCT_DEFINITION_SHAPE($,$,#56);
#3227=PRODUCT_DEFINITION_SHAPE($,$,#57);
#3228=PRODUCT_DEFINITION_SHAPE($,$,#58);
#3229=PRODUCT_DEFINITION_SHAPE($,$,#59);
#3230=PRODUCT_DEFINITION_SHAPE($,$,#60);
#3231=PRODUCT_DEFINITION_SHAPE($,$,#61);
#3232=PRODUCT_DEFINITION_SHAPE($,$,#62);
#3233=PRODUCT_DEFINITION_SHAPE($,$,#63);
#3234=PRODUCT_DEFINITION_SHAPE($,$,#64);
#3235=PRODUCT_DEFINITION_SHAPE($,$,#65);
#3236=PRODUCT_DEFINITION_SHAPE($,$,#66);
#3237=PRODUCT_DEFINITION_SHAPE($,$,#67);
#3238=PRODUCT_DEFINITION_SHAPE($,$,#68);
#3239=PRODUCT_DEFINITION_SHAPE($,$,#69);
#3240=PRODUCT_DEFINITION_SHAPE($,$,#70);
#3241=SHAPE_REPRESENTATION('',(#1353,#1503,#1504,#1505,#1506,#1507,#1508,
#1509,#1510,#1511,#1512,#1513,#1514,#1515,#1516,#1517),#3200);
#3242=SHAPE_REPRESENTATION('',(#1354),#3201);
#3243=SHAPE_REPRESENTATION('',(#1372),#3202);
#3244=SHAPE_REPRESENTATION('',(#1398),#3203);
#3245=SHAPE_REPRESENTATION('',(#1416),#3204);
#3246=SHAPE_REPRESENTATION('',(#1440),#3205);
#3247=SHAPE_REPRESENTATION('',(#1465),#3206);
#3248=PRODUCT_DEFINITION_CONTEXT('part definition',#3271,'design');
#3249=PRODUCT_DEFINITION('MAT-011','MAT-011',#3256,#3248);
#3250=PRODUCT_DEFINITION('Eye Bolt','Eye Bolt',#3257,#3248);
#3251=PRODUCT_DEFINITION('Pivot pin','Pivot Pin',#3258,#3248);
#3252=PRODUCT_DEFINITION('Axle Pin','Axle Pin',#3259,#3248);
#3253=PRODUCT_DEFINITION('Side plate','Side Plate',#3260,#3248);
#3254=PRODUCT_DEFINITION('Wheel','Wheel',#3261,#3248);
#3255=PRODUCT_DEFINITION('Hex Nut DIN Grade C','Hex Nut DIN Grade C',#3262,
#3248);
#3256=PRODUCT_DEFINITION_FORMATION('',$,#3273);
#3257=PRODUCT_DEFINITION_FORMATION('',$,#3274);
#3258=PRODUCT_DEFINITION_FORMATION('',$,#3275);
#3259=PRODUCT_DEFINITION_FORMATION('',$,#3276);
#3260=PRODUCT_DEFINITION_FORMATION('',$,#3277);
#3261=PRODUCT_DEFINITION_FORMATION('',$,#3278);
#3262=PRODUCT_DEFINITION_FORMATION('',$,#3279);
#3263=PRODUCT_RELATED_PRODUCT_CATEGORY('MAT-011','MAT-011',(#3273));
#3264=PRODUCT_RELATED_PRODUCT_CATEGORY('Eye Bolt','Eye Bolt',(#3274));
#3265=PRODUCT_RELATED_PRODUCT_CATEGORY('Pivot Pin','Pivot Pin',(#3275));
#3266=PRODUCT_RELATED_PRODUCT_CATEGORY('Axle Pin','Axle Pin',(#3276));
#3267=PRODUCT_RELATED_PRODUCT_CATEGORY('Side Plate','Side Plate',(#3277));
#3268=PRODUCT_RELATED_PRODUCT_CATEGORY('Wheel','Wheel',(#3278));
#3269=PRODUCT_RELATED_PRODUCT_CATEGORY('Hex Nut DIN Grade C',
'Hex Nut DIN Grade C',(#3279));
#3270=APPLICATION_PROTOCOL_DEFINITION('international standard',
'automotive_design',2009,#3271);
#3271=APPLICATION_CONTEXT(
'Core Data for Automotive Mechanical Design Process');
#3272=PRODUCT_CONTEXT('part definition',#3271,'mechanical');
#3273=PRODUCT('MAT-011','MAT-011','STEP AP214',(#3272));
#3274=PRODUCT('Eye Bolt','Eye Bolt',$,(#3272));
#3275=PRODUCT('Pivot pin','Pivot Pin','Pivot pin',(#3272));
#3276=PRODUCT('Axle Pin','Axle Pin',$,(#3272));
#3277=PRODUCT('Side plate','Side Plate','Side plate',(#3272));
#3278=PRODUCT('Wheel','Wheel','Wheel',(#3272));
#3279=PRODUCT('Hex Nut DIN Grade C','Hex Nut DIN Grade C',$,(#3272));
#3280=PRESENTATION_STYLE_ASSIGNMENT((#3284));
#3281=PRESENTATION_STYLE_ASSIGNMENT((#3285));
#3282=PRESENTATION_STYLE_ASSIGNMENT((#3286));
#3283=PRESENTATION_STYLE_ASSIGNMENT((#3287));
#3284=SURFACE_STYLE_USAGE(.BOTH.,#3288);
#3285=SURFACE_STYLE_USAGE(.BOTH.,#3289);
#3286=SURFACE_STYLE_USAGE(.BOTH.,#3290);
#3287=SURFACE_STYLE_USAGE(.BOTH.,#3291);
#3288=SURFACE_SIDE_STYLE('',(#3292));
#3289=SURFACE_SIDE_STYLE('',(#3293));
#3290=SURFACE_SIDE_STYLE('',(#3294));
#3291=SURFACE_SIDE_STYLE('',(#3295));
#3292=SURFACE_STYLE_FILL_AREA(#3296);
#3293=SURFACE_STYLE_FILL_AREA(#3297);
#3294=SURFACE_STYLE_FILL_AREA(#3298);
#3295=SURFACE_STYLE_FILL_AREA(#3299);
#3296=FILL_AREA_STYLE('Steel - Satin',(#3300));
#3297=FILL_AREA_STYLE('Opaque(97,158,199)',(#3301));
#3298=FILL_AREA_STYLE('Opaque(227,224,212)',(#3302));
#3299=FILL_AREA_STYLE('Opaque(31,36,43)',(#3303));
#3300=FILL_AREA_STYLE_COLOUR('Steel - Satin',#3304);
#3301=FILL_AREA_STYLE_COLOUR('Opaque(97,158,199)',#3305);
#3302=FILL_AREA_STYLE_COLOUR('Opaque(227,224,212)',#3306);
#3303=FILL_AREA_STYLE_COLOUR('Opaque(31,36,43)',#3307);
#3304=COLOUR_RGB('Steel - Satin',0.627450980392157,0.627450980392157,0.627450980392157);
#3305=COLOUR_RGB('Opaque(97,158,199)',0.380392156862745,0.619607843137255,
0.780392156862745);
#3306=COLOUR_RGB('Opaque(227,224,212)',0.890196078431372,0.87843137254902,
0.831372549019608);
#3307=COLOUR_RGB('Opaque(31,36,43)',0.12156862745098,0.141176470588235,
0.168627450980392);
ENDSEC;
END-ISO-10303-21;
